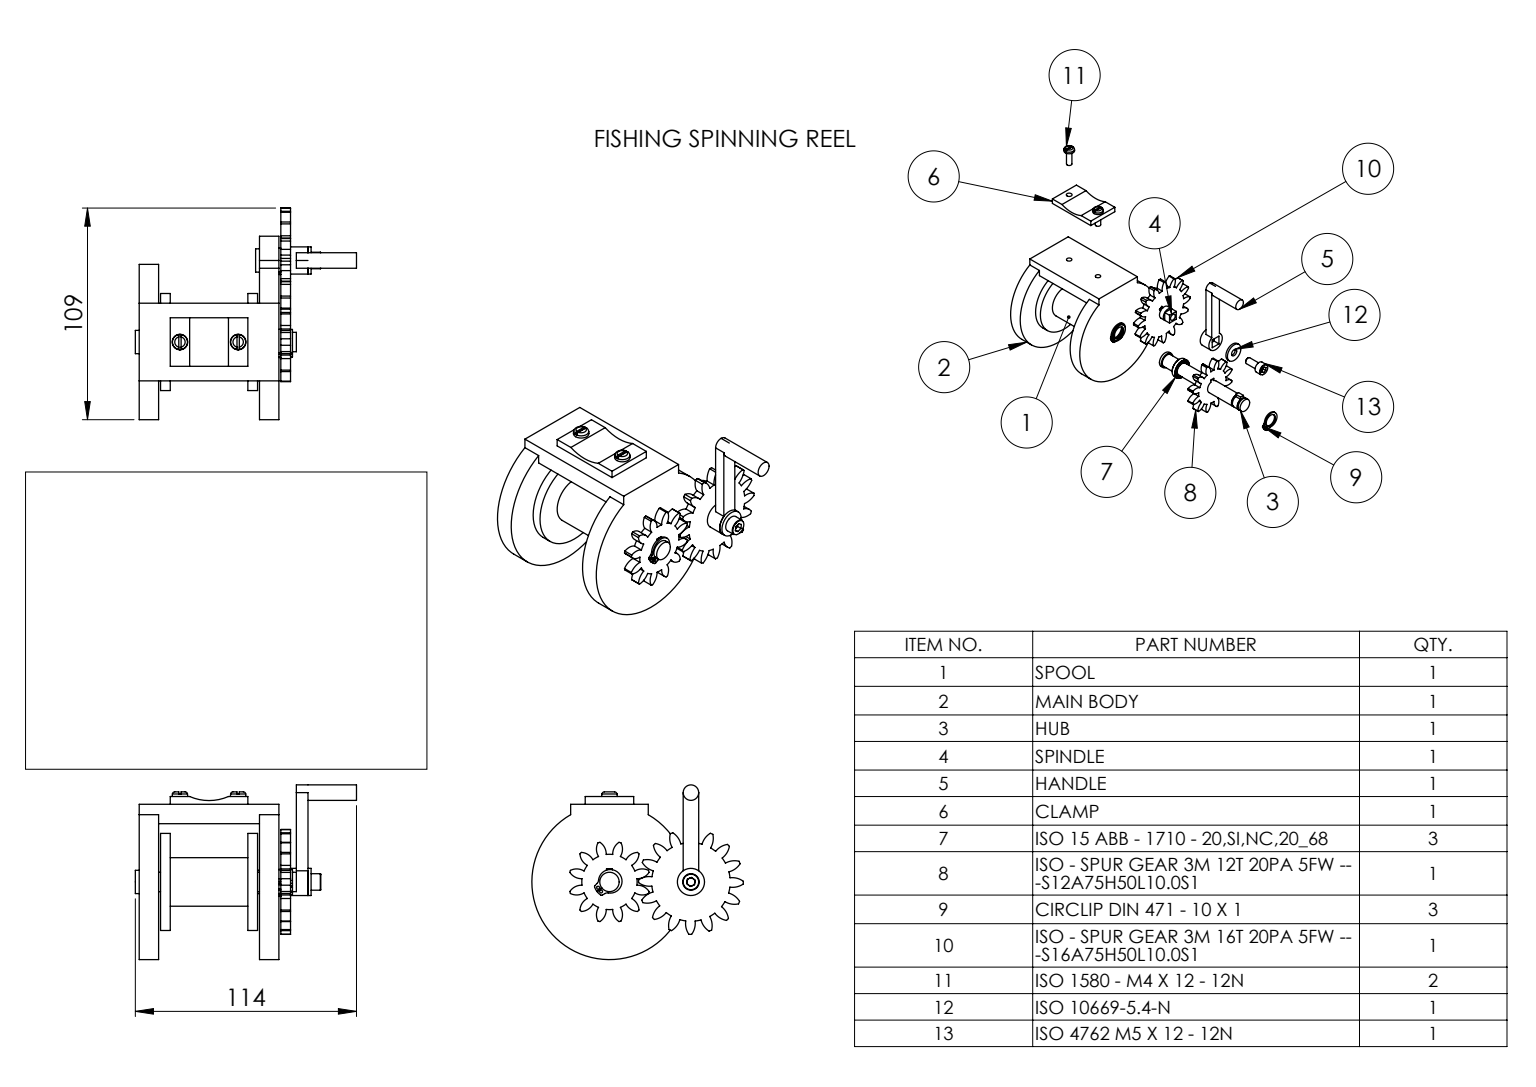
ISO-10303-21;
HEADER;
FILE_DESCRIPTION (('STEP AP214'),
    '1' );
FILE_NAME ('MAS-168',
    '2026-10-27T08:02:39',
    ( '' ),
    ( '' ),
    'SwSTEP 2.0',
    'SolidWorks 2026',
    '' );
FILE_SCHEMA (( 'AUTOMOTIVE_DESIGN' ));
ENDSEC;

DATA;
#1 = CARTESIAN_POINT ( 'NONE',  ( 4.999999999999999112, 8.035066368449411911, -14.88411597386720508 ) ) ;
#2 = FACE_OUTER_BOUND ( 'NONE', #4897, .T. ) ;
#3 = AXIS2_PLACEMENT_3D ( 'NONE', #7464, #2948, #5642 ) ;
#4 = AXIS2_PLACEMENT_3D ( 'NONE', #1352, #1240, #9072 ) ;
#5 = CARTESIAN_POINT ( 'NONE',  ( 0.000000000000000000, -11.14352537685160982, -19.60720892790264713 ) ) ;
#6 = PLANE ( 'NONE',  #3841 ) ;
#7 = ORIENTED_EDGE ( 'NONE', *, *, #8174, .F. ) ;
#8 = CYLINDRICAL_SURFACE ( 'NONE', #3786, 14.24900000001425227 ) ;
#9 = CARTESIAN_POINT ( 'NONE',  ( -36.00100000000000477, 0.000000000000000000, -41.99999999999999289 ) ) ;
#10 = ORIENTED_EDGE ( 'NONE', *, *, #7633, .F. ) ;
#11 = LINE ( 'NONE', #10463, #885 ) ;
#12 = UNCERTAINTY_MEASURE_WITH_UNIT (LENGTH_MEASURE( 1.000000000000000082E-05 ), #6900, 'distance_accuracy_value', 'NONE');
#13 = ORIENTED_EDGE ( 'NONE', *, *, #11735, .F. ) ;
#14 = CIRCLE ( 'NONE', #9018, 40.00000000000000711 ) ;
#15 = AXIS2_PLACEMENT_3D ( 'NONE', #471, #2401, #339 ) ;
#16 = EDGE_CURVE ( 'NONE', #8654, #9068, #398, .T. ) ;
#17 = SURFACE_STYLE_FILL_AREA ( #6591 ) ;
#18 = APPLICATION_CONTEXT ( 'automotive_design' ) ;
#19 = DIRECTION ( 'NONE',  ( -0.000000000000000000, 1.000000000000000000, -0.000000000000000000 ) ) ;
#20 = CARTESIAN_POINT ( 'NONE',  ( 0.000000000000000000, 0.000000000000000000, 0.000000000000000000 ) ) ;
#21 =( GEOMETRIC_REPRESENTATION_CONTEXT ( 3 ) GLOBAL_UNCERTAINTY_ASSIGNED_CONTEXT ( ( #3529 ) ) GLOBAL_UNIT_ASSIGNED_CONTEXT ( ( #3001, #9758, #2180 ) ) REPRESENTATION_CONTEXT ( 'NONE', 'WORKASPACE' ) );
#22 = DIRECTION ( 'NONE',  ( -1.000000000000000000, 0.000000000000000000, 0.000000000000000000 ) ) ;
#23 = FACE_BOUND ( 'NONE', #5725, .T. ) ;
#24 = AXIS2_PLACEMENT_3D ( 'NONE', #11957, #9116, #6050 ) ;
#25 = CIRCLE ( 'NONE', #9413, 20.24900000002024925 ) ;
#26 = VERTEX_POINT ( 'NONE', #5218 ) ;
#27 = EDGE_LOOP ( 'NONE', ( #3716, #7736, #9091, #8420 ) ) ;
#28 = VECTOR ( 'NONE', #1970, 1000.000000000000000 ) ;
#29 = CYLINDRICAL_SURFACE ( 'NONE', #9817, 4.799999999999999822 ) ;
#30 = AXIS2_PLACEMENT_3D ( 'NONE', #1488, #11904, #1413 ) ;
#31 = VERTEX_POINT ( 'NONE', #9797 ) ;
#32 = DIRECTION ( 'NONE',  ( 1.000000000000000000, -0.000000000000000000, 0.000000000000000000 ) ) ;
#33 = SHAPE_DEFINITION_REPRESENTATION ( #1615, #7946 ) ;
#34 = ORIENTED_EDGE ( 'NONE', *, *, #1883, .F. ) ;
#35 = ADVANCED_FACE ( 'NONE', ( #6155 ), #7977, .T. ) ;
#36 = AXIS2_PLACEMENT_3D ( 'NONE', #6295, #7112, #8236 ) ;
#37 = VECTOR ( 'NONE', #10938, 1000.000000000000000 ) ;
#38 = EDGE_CURVE ( 'NONE', #10710, #279, #12151, .T. ) ;
#39 = AXIS2_PLACEMENT_3D ( 'NONE', #8335, #2568, #9339 ) ;
#40 = ORIENTED_EDGE ( 'NONE', *, *, #10982, .T. ) ;
#41 = AXIS2_PLACEMENT_3D ( 'NONE', #9780, #4085, #382 ) ;
#42 = EDGE_CURVE ( 'NONE', #9980, #7044, #6787, .T. ) ;
#43 = ORIENTED_EDGE ( 'NONE', *, *, #3948, .F. ) ;
#44 = CARTESIAN_POINT ( 'NONE',  ( 4.999999999999999112, 22.37914155802281257, 2.791921004064645384 ) ) ;
#45 = DIRECTION ( 'NONE',  ( 0.03086419753086420623, -0.9995235871707959241, 0.000000000000000000 ) ) ;
#46 = DIRECTION ( 'NONE',  ( 0.000000000000000000, 0.000000000000000000, -1.000000000000000000 ) ) ;
#47 = DIRECTION ( 'NONE',  ( 0.000000000000000000, 0.000000000000000000, -1.000000000000000000 ) ) ;
#48 = ORIENTED_EDGE ( 'NONE', *, *, #3948, .T. ) ;
#50 = CYLINDRICAL_SURFACE ( 'NONE', #10960, 20.24900000002024569 ) ;
#49 =( GEOMETRIC_REPRESENTATION_CONTEXT ( 3 ) GLOBAL_UNCERTAINTY_ASSIGNED_CONTEXT ( ( #7777 ) ) GLOBAL_UNIT_ASSIGNED_CONTEXT ( ( #2594, #966, #4784 ) ) REPRESENTATION_CONTEXT ( 'NONE', 'WORKASPACE' ) );
#51 = CIRCLE ( 'NONE', #4842, 5.525000000000000355 ) ;
#52 = ORIENTED_EDGE ( 'NONE', *, *, #6778, .T. ) ;
#53 = CIRCLE ( 'NONE', #7047, 9.600000000009602630 ) ;
#54 = CIRCLE ( 'NONE', #10234, 3.873645755336797780 ) ;
#55 = ORIENTED_EDGE ( 'NONE', *, *, #1807, .F. ) ;
#56 = DIRECTION ( 'NONE',  ( 1.000000000000000000, 0.000000000000000000, 0.000000000000000000 ) ) ;
#57 = ORIENTED_EDGE ( 'NONE', *, *, #11975, .F. ) ;
#58 = DIRECTION ( 'NONE',  ( 0.000000000000000000, 0.000000000000000000, -1.000000000000000000 ) ) ;
#59 = ADVANCED_FACE ( 'NONE', ( #10781 ), #4214, .F. ) ;
#60 = EDGE_CURVE ( 'NONE', #6322, #1163, #6180, .T. ) ;
#61 = AXIS2_PLACEMENT_3D ( 'NONE', #4536, #722, #776 ) ;
#62 = VECTOR ( 'NONE', #7382, 1000.000000000000000 ) ;
#63 = EDGE_CURVE ( 'NONE', #1039, #8590, #3790, .T. ) ;
#64 = VECTOR ( 'NONE', #5535, 1000.000000000000000 ) ;
#65 = DIRECTION ( 'NONE',  ( 0.000000000000000000, 0.6828850436591804574, 0.7305258497456468270 ) ) ;
#66 = VECTOR ( 'NONE', #9457, 1000.000000000000000 ) ;
#67 = DIRECTION ( 'NONE',  ( 0.000000000000000000, 0.000000000000000000, -1.000000000000000000 ) ) ;
#68 = DIRECTION ( 'NONE',  ( -1.000000000000000000, -3.903127820947815962E-18, 0.000000000000000000 ) ) ;
#69 = ORIENTED_EDGE ( 'NONE', *, *, #8618, .F. ) ;
#70 = LINE ( 'NONE', #2883, #8880 ) ;
#71 =( LENGTH_UNIT ( ) NAMED_UNIT ( * ) SI_UNIT ( .MILLI., .METRE. ) );
#72 = CARTESIAN_POINT ( 'NONE',  ( 0.000000000000000000, -20.13931372320393010, 5.950465759858794002 ) ) ;
#73 = CARTESIAN_POINT ( 'NONE',  ( 37.00000000000000711, 6.799999999999998046, 1.500000000000000000 ) ) ;
#74 = EDGE_CURVE ( 'NONE', #10051, #9763, #2189, .T. ) ;
#75 = AXIS2_PLACEMENT_3D ( 'NONE', #10633, #5941, #1246 ) ;
#76 = ORIENTED_EDGE ( 'NONE', *, *, #9297, .F. ) ;
#77 = FACE_BOUND ( 'NONE', #651, .T. ) ;
#78 = EDGE_CURVE ( 'NONE', #474, #1066, #6869, .T. ) ;
#79 = DIRECTION ( 'NONE',  ( -1.000000000000000000, 0.000000000000000000, 0.000000000000000000 ) ) ;
#80 = CARTESIAN_POINT ( 'NONE',  ( 50.00005079999999680, 0.000000000000000000, 5.000000000000000000 ) ) ;
#81 = CARTESIAN_POINT ( 'NONE',  ( 2.499999999999999556, 22.05152472667151642, -15.57980286237449619 ) ) ;
#82 = EDGE_LOOP ( 'NONE', ( #2699, #3221, #1279, #723 ) ) ;
#83 = LINE ( 'NONE', #947, #2363 ) ;
#84 = CARTESIAN_POINT ( 'NONE',  ( 36.00000000000000711, -3.606021680338235225, -38.83193945118931367 ) ) ;
#85 = EDGE_LOOP ( 'NONE', ( #11656, #7986, #6514, #6024 ) ) ;
#86 = DIRECTION ( 'NONE',  ( 1.000000000000000000, -0.000000000000000000, -0.000000000000000000 ) ) ;
#87 = EDGE_CURVE ( 'NONE', #5401, #10239, #7657, .T. ) ;
#88 = VERTEX_POINT ( 'NONE', #10671 ) ;
#89 = AXIS2_PLACEMENT_3D ( 'NONE', #7473, #7293, #11207 ) ;
#90 = DIRECTION ( 'NONE',  ( -1.000000000000000000, -0.000000000000000000, -0.000000000000000000 ) ) ;
#91 = CARTESIAN_POINT ( 'NONE',  ( 3.098410542199072637, -7.060458129626440815, -1.000000000000000000 ) ) ;
#92 = DIRECTION ( 'NONE',  ( 1.000000000000000000, -0.000000000000000000, -0.000000000000000000 ) ) ;
#93 = CARTESIAN_POINT ( 'NONE',  ( 26.00000000000000355, 0.000000000000000000, -41.99999999999999289 ) ) ;
#94 = EDGE_LOOP ( 'NONE', ( #11994, #4647, #11472, #6806 ) ) ;
#95 = ORIENTED_EDGE ( 'NONE', *, *, #5318, .F. ) ;
#96 = VECTOR ( 'NONE', #10392, 1000.000000000000000 ) ;
#97 =( NAMED_UNIT ( * ) SI_UNIT ( $, .STERADIAN. ) SOLID_ANGLE_UNIT ( ) );
#98 = ORIENTED_EDGE ( 'NONE', *, *, #8688, .T. ) ;
#99 = DIRECTION ( 'NONE',  ( 0.000000000000000000, 0.6828850436591804574, 0.7305258497456468270 ) ) ;
#100 = PRODUCT_CONTEXT ( 'NONE', #11984, 'mechanical' ) ;
#101 = EDGE_LOOP ( 'NONE', ( #11163, #3779, #6204, #11294 ) ) ;
#102 = VERTEX_POINT ( 'NONE', #11771 ) ;
#103 = VERTEX_POINT ( 'NONE', #3228 ) ;
#104 = DIRECTION ( 'NONE',  ( -1.000000000000000000, -0.000000000000000000, 0.000000000000000000 ) ) ;
#105 = LINE ( 'NONE', #3865, #7814 ) ;
#106 = CARTESIAN_POINT ( 'NONE',  ( -31.74999999999995737, 5.204748896376250699E-16, -4.250000000000000000 ) ) ;
#107 = DIRECTION ( 'NONE',  ( -1.000000000000000000, 0.000000000000000000, -0.000000000000000000 ) ) ;
#108 = EDGE_CURVE ( 'NONE', #8484, #432, #5151, .T. ) ;
#109 = ORIENTED_EDGE ( 'NONE', *, *, #4761, .F. ) ;
#110 = FACE_OUTER_BOUND ( 'NONE', #7615, .T. ) ;
#111 = EDGE_LOOP ( 'NONE', ( #11683, #9345, #10603, #11669 ) ) ;
#112 = ADVANCED_FACE ( 'NONE', ( #8980 ), #4043, .T. ) ;
#113 = SURFACE_STYLE_FILL_AREA ( #10791 ) ;
#114 = VERTEX_POINT ( 'NONE', #4279 ) ;
#115 = CARTESIAN_POINT ( 'NONE',  ( -26.00000000000000355, -4.898587196589413815E-15, -40.00000000000000711 ) ) ;
#116 = ORIENTED_EDGE ( 'NONE', *, *, #4223, .F. ) ;
#117 = DIRECTION ( 'NONE',  ( 0.000000000000000000, 0.000000000000000000, 1.000000000000000000 ) ) ;
#118 = CARTESIAN_POINT ( 'NONE',  ( 2.500000000000000000, -1.178949249685213863, 2.042000000000002924 ) ) ;
#119 = EDGE_CURVE ( 'NONE', #4367, #3187, #6988, .T. ) ;
#120 = EDGE_LOOP ( 'NONE', ( #9318, #12086, #3898, #6255 ) ) ;
#121 = DIRECTION ( 'NONE',  ( 0.000000000000000000, 0.000000000000000000, 1.000000000000000000 ) ) ;
#122 = DIRECTION ( 'NONE',  ( -1.000000000000000000, 0.000000000000000000, 0.000000000000000000 ) ) ;
#123 = ORIENTED_EDGE ( 'NONE', *, *, #7333, .T. ) ;
#124 = DIRECTION ( 'NONE',  ( 0.000000000000000000, 0.000000000000000000, 1.000000000000000000 ) ) ;
#125 = EDGE_CURVE ( 'NONE', #9327, #10148, #1383, .T. ) ;
#126 = CARTESIAN_POINT ( 'NONE',  ( 0.000000000000000000, 20.13931372320388391, 5.950465759858938775 ) ) ;
#127 = EDGE_CURVE ( 'NONE', #10133, #6749, #9113, .T. ) ;
#128 = EDGE_CURVE ( 'NONE', #10292, #8107, #5580, .T. ) ;
#129 = DIRECTION ( 'NONE',  ( -1.000000000000000000, -0.000000000000000000, -0.000000000000000000 ) ) ;
#130 = VERTEX_POINT ( 'NONE', #2582 ) ;
#131 = CARTESIAN_POINT ( 'NONE',  ( 29.00000000000000000, 9.184850993605147944E-16, -49.49999999999999289 ) ) ;
#132 = PRODUCT ( 'circlip for shafts normal_din_Circlip DIN 471 - 10 x 1', 'circlip for shafts normal_din_Circlip DIN 471 - 10 x 1', '', ( #2666 ) ) ;
#133 = DIRECTION ( 'NONE',  ( -1.000000000000000000, -0.000000000000000000, -0.000000000000000000 ) ) ;
#134 = LINE ( 'NONE', #5901, #805 ) ;
#135 = EDGE_CURVE ( 'NONE', #9980, #9876, #10102, .T. ) ;
#136 = LINE ( 'NONE', #11503, #10649 ) ;
#137 = LINE ( 'NONE', #2829, #1850 ) ;
#138 = VERTEX_POINT ( 'NONE', #7349 ) ;
#139 = DIRECTION ( 'NONE',  ( 0.000000000000000000, 0.000000000000000000, 1.000000000000000000 ) ) ;
#140 = DIRECTION ( 'NONE',  ( 1.000000000000000000, 0.000000000000000000, 0.000000000000000000 ) ) ;
#141 = ORIENTED_EDGE ( 'NONE', *, *, #8217, .F. ) ;
#142 = FACE_BOUND ( 'NONE', #771, .T. ) ;
#143 = UNCERTAINTY_MEASURE_WITH_UNIT (LENGTH_MEASURE( 1.000000000000000082E-05 ), #8122, 'distance_accuracy_value', 'NONE');
#144 = ORIENTED_EDGE ( 'NONE', *, *, #7851, .F. ) ;
#145 = DIRECTION ( 'NONE',  ( 0.000000000000000000, 0.000000000000000000, -1.000000000000000000 ) ) ;
#146 = FACE_OUTER_BOUND ( 'NONE', #6316, .T. ) ;
#147 = EDGE_CURVE ( 'NONE', #5793, #9690, #7785, .T. ) ;
#148 = EDGE_CURVE ( 'NONE', #6125, #9230, #7162, .T. ) ;
#149 = DIRECTION ( 'NONE',  ( 0.000000000000000000, 0.000000000000000000, 1.000000000000000000 ) ) ;
#150 = DIRECTION ( 'NONE',  ( 1.000000000000000000, 0.000000000000000000, 0.000000000000000000 ) ) ;
#151 = ORIENTED_EDGE ( 'NONE', *, *, #5543, .T. ) ;
#152 = ORIENTED_EDGE ( 'NONE', *, *, #2116, .F. ) ;
#153 = EDGE_LOOP ( 'NONE', ( #1044, #6924 ) ) ;
#154 = SURFACE_STYLE_USAGE ( .BOTH. , #911 ) ;
#155 = SHAPE_DEFINITION_REPRESENTATION ( #437, #678 ) ;
#156 = ORIENTED_EDGE ( 'NONE', *, *, #8748, .T. ) ;
#157 = ORIENTED_EDGE ( 'NONE', *, *, #3999, .F. ) ;
#158 = ORIENTED_EDGE ( 'NONE', *, *, #10534, .F. ) ;
#159 = PLANE ( 'NONE',  #4576 ) ;
#160 = FACE_OUTER_BOUND ( 'NONE', #3496, .T. ) ;
#161 = CARTESIAN_POINT ( 'NONE',  ( 0.000000000000000000, 0.000000000000000000, 0.000000000000000000 ) ) ;
#162 = DIRECTION ( 'NONE',  ( 1.000000000000000000, 0.000000000000000000, 0.000000000000000000 ) ) ;
#163 = ORIENTED_EDGE ( 'NONE', *, *, #2128, .T. ) ;
#164 = CARTESIAN_POINT ( 'NONE',  ( 10.00000000000000000, 44.00000000000001421, -12.50000000000000000 ) ) ;
#165 = EDGE_LOOP ( 'NONE', ( #11428, #11250, #3782, #590 ) ) ;
#166 = EDGE_LOOP ( 'NONE', ( #4533, #1972 ) ) ;
#168 = DIRECTION ( 'NONE',  ( 0.000000000000000000, 0.000000000000000000, 1.000000000000000000 ) ) ;
#167 = AXIS2_PLACEMENT_3D ( 'NONE', #171, #5883, #6935 ) ;
#169 = CIRCLE ( 'NONE', #368, 3.873645755336797780 ) ;
#170 = VERTEX_POINT ( 'NONE', #7231 ) ;
#171 = CARTESIAN_POINT ( 'NONE',  ( 1.500000000000001332, 0.000000000000000000, 0.000000000000000000 ) ) ;
#172 = VECTOR ( 'NONE', #10661, 1000.000000000000000 ) ;
#173 = CARTESIAN_POINT ( 'NONE',  ( 2.500000000000000000, -1.768423874527823791, -1.020999999999998353 ) ) ;
#174 = EDGE_CURVE ( 'NONE', #11053, #10042, #2785, .T. ) ;
#175 = CIRCLE ( 'NONE', #11932, 27.00000000002699707 ) ;
#176 = ORIENTED_EDGE ( 'NONE', *, *, #434, .T. ) ;
#177 = CLOSED_SHELL ( 'NONE', ( #10284, #2336, #8766, #4424, #8491, #9078, #4920, #2783, #9249, #727, #1702, #2014, #7994, #8544, #7366, #12201, #5608, #5505, #10582, #11708, #6045, #8749, #2274, #6335, #7524, #5095, #6706, #112, #3625, #728, #7634, #6314, #6863, #8461, #9912, #6936, #3075, #7445, #11950, #5150, #5319, #7411, #10495, #2256, #1343, #9815, #12107, #8150, #5564, #11571, #10132, #3776, #7922, #4726, #8290, #2161, #3112, #11868, #8305, #4757, #8516, #1346, #525, #10969, #10935, #8135, #12114, #7185, #9760, #8007, #2667, #5107, #4369, #5486, #6938, #820, #1296 ) ) ;
#178 = DIRECTION ( 'NONE',  ( -1.000000000000000000, 0.000000000000000000, 0.000000000000000000 ) ) ;
#179 = DIRECTION ( 'NONE',  ( 0.000000000000000000, 0.000000000000000000, 1.000000000000000000 ) ) ;
#180 = ORIENTED_EDGE ( 'NONE', *, *, #4930, .T. ) ;
#181 = CYLINDRICAL_SURFACE ( 'NONE', #468, 5.000000000000004441 ) ;
#182 = SURFACE_STYLE_USAGE ( .BOTH. , #5944 ) ;
#183 = CARTESIAN_POINT ( 'NONE',  ( 0.000000000000000000, -22.05152472667118957, -15.57980286237495626 ) ) ;
#184 = DIRECTION ( 'NONE',  ( 1.000000000000000000, 0.000000000000000000, 0.000000000000000000 ) ) ;
#185 = VERTEX_POINT ( 'NONE', #1476 ) ;
#186 = FACE_OUTER_BOUND ( 'NONE', #7398, .T. ) ;
#187 = VECTOR ( 'NONE', #9799, 999.9999999999998863 ) ;
#188 = CIRCLE ( 'NONE', #6974, 7.500000000000000888 ) ;
#189 = EDGE_CURVE ( 'NONE', #3572, #7704, #8788, .T. ) ;
#190 = AXIS2_PLACEMENT_3D ( 'NONE', #3113, #5922, #4971 ) ;
#191 = EDGE_CURVE ( 'NONE', #922, #11041, #11147, .T. ) ;
#192 = EDGE_CURVE ( 'NONE', #3603, #3952, #2381, .T. ) ;
#193 = DIRECTION ( 'NONE',  ( -1.000000000000000000, -0.000000000000000000, -0.000000000000000000 ) ) ;
#194 = CARTESIAN_POINT ( 'NONE',  ( 51.00000000000000000, -3.499999999999998668, -45.49999999999998579 ) ) ;
#195 = DIRECTION ( 'NONE',  ( 0.000000000000000000, 0.000000000000000000, 1.000000000000000000 ) ) ;
#196 = DIRECTION ( 'NONE',  ( 0.000000000000000000, 0.000000000000000000, 1.000000000000000000 ) ) ;
#197 = CIRCLE ( 'NONE', #11173, 2.000000000000000000 ) ;
#198 = EDGE_LOOP ( 'NONE', ( #4927, #6870, #4753, #5176, #4314 ) ) ;
#199 = DIRECTION ( 'NONE',  ( -1.000000000000000000, -0.000000000000000000, 0.000000000000000000 ) ) ;
#200 = DIRECTION ( 'NONE',  ( 0.000000000000000000, 0.000000000000000000, 1.000000000000000000 ) ) ;
#201 = AXIS2_PLACEMENT_3D ( 'NONE', #9324, #9448, #3624 ) ;
#202 = ORIENTED_EDGE ( 'NONE', *, *, #9372, .F. ) ;
#203 = CYLINDRICAL_SURFACE ( 'NONE', #8088, 7.500000000000000000 ) ;
#204 = ORIENTED_EDGE ( 'NONE', *, *, #38, .F. ) ;
#205 = DIRECTION ( 'NONE',  ( 0.000000000000000000, 0.000000000000000000, 1.000000000000000000 ) ) ;
#206 = VECTOR ( 'NONE', #6495, 1000.000000000000000 ) ;
#207 = DIRECTION ( 'NONE',  ( 1.000000000000000000, 0.000000000000000000, 0.000000000000000000 ) ) ;
#208 = CARTESIAN_POINT ( 'NONE',  ( 0.000000000000000000, -5.984728032765115557, 21.74405275335756116 ) ) ;
#209 = DIRECTION ( 'NONE',  ( 0.000000000000000000, 1.224646799147353207E-16, 1.000000000000000000 ) ) ;
#210 = CARTESIAN_POINT ( 'NONE',  ( 4.999999999999999112, -16.90755573046745752, -0.4834863907627537372 ) ) ;
#211 = ORIENTED_EDGE ( 'NONE', *, *, #8369, .F. ) ;
#212 = CARTESIAN_POINT ( 'NONE',  ( 0.000000000000000000, 0.000000000000000000, 0.000000000000000000 ) ) ;
#213 = CIRCLE ( 'NONE', #1019, 7.500000000000000888 ) ;
#214 = VERTEX_POINT ( 'NONE', #5344 ) ;
#215 = FACE_OUTER_BOUND ( 'NONE', #11653, .T. ) ;
#216 = AXIS2_PLACEMENT_3D ( 'NONE', #497, #4306, #3323 ) ;
#217 = ORIENTED_EDGE ( 'NONE', *, *, #2945, .T. ) ;
#218 = CIRCLE ( 'NONE', #406, 7.200000000007204193 ) ;
#219 = ADVANCED_FACE ( 'NONE', ( #2468 ), #6409, .F. ) ;
#220 = ADVANCED_FACE ( 'NONE', ( #5475 ), #2655, .F. ) ;
#221 = DIRECTION ( 'NONE',  ( -1.000000000000000000, -0.000000000000000000, -0.000000000000000000 ) ) ;
#222 = AXIS2_PLACEMENT_3D ( 'NONE', #3797, #9085, #2730 ) ;
#223 = ORIENTED_EDGE ( 'NONE', *, *, #8092, .T. ) ;
#224 = AXIS2_PLACEMENT_3D ( 'NONE', #1139, #4013, #1014 ) ;
#225 = FACE_OUTER_BOUND ( 'NONE', #3091, .T. ) ;
#226 = DIRECTION ( 'NONE',  ( 1.000000000000000000, 0.000000000000000000, 0.000000000000000000 ) ) ;
#227 = CIRCLE ( 'NONE', #1419, 14.24900000001425227 ) ;
#228 = AXIS2_PLACEMENT_3D ( 'NONE', #6814, #4871, #168 ) ;
#229 = LINE ( 'NONE', #3922, #9820 ) ;
#230 = CYLINDRICAL_SURFACE ( 'NONE', #1227, 7.200000000007202416 ) ;
#231 = VERTEX_POINT ( 'NONE', #3477 ) ;
#232 = ORIENTED_EDGE ( 'NONE', *, *, #10676, .F. ) ;
#233 =( NAMED_UNIT ( * ) SI_UNIT ( $, .STERADIAN. ) SOLID_ANGLE_UNIT ( ) );
#234 = ORIENTED_EDGE ( 'NONE', *, *, #9201, .F. ) ;
#235 = AXIS2_PLACEMENT_3D ( 'NONE', #1289, #9923, #1479 ) ;
#236 = DIRECTION ( 'NONE',  ( -1.000000000000000000, -3.903127820947815962E-18, 0.000000000000000000 ) ) ;
#237 = AXIS2_PLACEMENT_3D ( 'NONE', #4529, #4405, #8346 ) ;
#238 = VERTEX_POINT ( 'NONE', #12026 ) ;
#239 = DIRECTION ( 'NONE',  ( -1.000000000000000000, 0.000000000000000000, 0.000000000000000000 ) ) ;
#240 = AXIS2_PLACEMENT_3D ( 'NONE', #7909, #5962, #9852 ) ;
#241 = CARTESIAN_POINT ( 'NONE',  ( 0.000000000000000000, -21.74405275335762155, 15.58472803277448726 ) ) ;
#242 = VECTOR ( 'NONE', #2897, 1000.000000000000000 ) ;
#243 = CONICAL_SURFACE ( 'NONE', #4238, 2.500000000000002220, 1.029744260000000189 ) ;
#244 = ORIENTED_EDGE ( 'NONE', *, *, #2101, .F. ) ;
#245 = CIRCLE ( 'NONE', #10429, 20.24900000002024569 ) ;
#246 = DIRECTION ( 'NONE',  ( -1.000000000000000000, -0.000000000000000000, -0.000000000000000000 ) ) ;
#247 = DIRECTION ( 'NONE',  ( 0.000000000000000000, 0.000000000000000000, -1.000000000000000000 ) ) ;
#248 = ORIENTED_EDGE ( 'NONE', *, *, #430, .T. ) ;
#249 = FACE_OUTER_BOUND ( 'NONE', #9270, .T. ) ;
#250 = FILL_AREA_STYLE ('',( #6001 ) ) ;
#251 = LINE ( 'NONE', #9999, #3639 ) ;
#252 = DIRECTION ( 'NONE',  ( 0.000000000000000000, 0.000000000000000000, -1.000000000000000000 ) ) ;
#253 = EDGE_LOOP ( 'NONE', ( #7852, #10617, #12284, #5866 ) ) ;
#254 = DIRECTION ( 'NONE',  ( 0.000000000000000000, 0.000000000000000000, 1.000000000000000000 ) ) ;
#255 = PRODUCT_DEFINITION_FORMATION_WITH_SPECIFIED_SOURCE ( 'ANY', '', #5718, .NOT_KNOWN. ) ;
#256 = VECTOR ( 'NONE', #8139, 1000.000000000000000 ) ;
#257 = AXIS2_PLACEMENT_3D ( 'NONE', #8422, #11402, #2776 ) ;
#258 = AXIS2_PLACEMENT_3D ( 'NONE', #11179, #11120, #1690 ) ;
#259 = MANIFOLD_SOLID_BREP ( 'Cavity1', #4172 ) ;
#260 = CARTESIAN_POINT ( 'NONE',  ( -36.00000000000000000, 0.000000000000000000, 0.000000000000000000 ) ) ;
#261 = CARTESIAN_POINT ( 'NONE',  ( 14.39999999999999680, 0.000000000000000000, 0.000000000000000000 ) ) ;
#262 = DIRECTION ( 'NONE',  ( -1.000000000000000000, 0.000000000000000000, 0.000000000000000000 ) ) ;
#263 = DIRECTION ( 'NONE',  ( -1.000000000000000000, 0.000000000000000000, 0.000000000000000000 ) ) ;
#264 = ORIENTED_EDGE ( 'NONE', *, *, #11856, .T. ) ;
#265 = EDGE_CURVE ( 'NONE', #8484, #2318, #5290, .T. ) ;
#266 = CARTESIAN_POINT ( 'NONE',  ( 0.000000000000000000, 22.83261415639523406, -14.41081992069285000 ) ) ;
#267 = VECTOR ( 'NONE', #3186, 1000.000000000000114 ) ;
#268 = LINE ( 'NONE', #2137, #3626 ) ;
#269 = ORIENTED_EDGE ( 'NONE', *, *, #579, .F. ) ;
#270 = CARTESIAN_POINT ( 'NONE',  ( 25.00000000000000000, 0.000000000000000000, 0.000000000000000000 ) ) ;
#271 = ADVANCED_FACE ( 'NONE', ( #5585 ), #7380, .T. ) ;
#272 = ORIENTED_EDGE ( 'NONE', *, *, #2387, .T. ) ;
#273 = PLANE ( 'NONE',  #1206 ) ;
#274 = AXIS2_PLACEMENT_3D ( 'NONE', #11157, #11099, #1724 ) ;
#275 = CYLINDRICAL_SURFACE ( 'NONE', #8197, 9.600000000009600853 ) ;
#276 = DIRECTION ( 'NONE',  ( 0.000000000000000000, 0.000000000000000000, 1.000000000000000000 ) ) ;
#277 = CARTESIAN_POINT ( 'NONE',  ( 0.000000000000000000, 46.00000000000001421, -41.99999999999999289 ) ) ;
#278 = FACE_OUTER_BOUND ( 'NONE', #10185, .T. ) ;
#279 = VERTEX_POINT ( 'NONE', #954 ) ;
#280 = MANIFOLD_SOLID_BREP ( 'Slot', #7978 ) ;
#281 = ORIENTED_EDGE ( 'NONE', *, *, #4388, .F. ) ;
#282 = FACE_BOUND ( 'NONE', #6825, .T. ) ;
#283 = EDGE_CURVE ( 'NONE', #6930, #9343, #6993, .T. ) ;
#284 = CIRCLE ( 'NONE', #2474, 4.800000000000000711 ) ;
#285 = EDGE_CURVE ( 'NONE', #11604, #9414, #8392, .T. ) ;
#286 = ORIENTED_EDGE ( 'NONE', *, *, #128, .F. ) ;
#287 = ADVANCED_FACE ( 'NONE', ( #2841 ), #4660, .F. ) ;
#288 = ORIENTED_EDGE ( 'NONE', *, *, #12313, .F. ) ;
#289 = ORIENTED_EDGE ( 'NONE', *, *, #4474, .F. ) ;
#290 = CARTESIAN_POINT ( 'NONE',  ( -1.250000000000000000, -6.429618962271402616, -1.000000000000000000 ) ) ;
#291 = DIRECTION ( 'NONE',  ( 0.000000000000000000, 0.000000000000000000, -1.000000000000000000 ) ) ;
#292 = CIRCLE ( 'NONE', #1490, 14.24900000001425582 ) ;
#293 = PLANE ( 'NONE',  #3827 ) ;
#294 = DIRECTION ( 'NONE',  ( 0.000000000000000000, 0.000000000000000000, -1.000000000000000000 ) ) ;
#295 = EDGE_LOOP ( 'NONE', ( #1962, #11859, #3381, #7606 ) ) ;
#296 = EDGE_CURVE ( 'NONE', #558, #1455, #8477, .T. ) ;
#297 = EDGE_LOOP ( 'NONE', ( #11234, #9949, #2749, #9847 ) ) ;
#298 = ORIENTED_EDGE ( 'NONE', *, *, #9479, .T. ) ;
#299 = FACE_OUTER_BOUND ( 'NONE', #4000, .T. ) ;
#300 = CIRCLE ( 'NONE', #2904, 21.00000000002100009 ) ;
#301 = DIRECTION ( 'NONE',  ( -1.000000000000000000, 0.000000000000000000, -0.000000000000000000 ) ) ;
#302 = FACE_OUTER_BOUND ( 'NONE', #521, .T. ) ;
#303 = VERTEX_POINT ( 'NONE', #4769 ) ;
#304 = AXIS2_PLACEMENT_3D ( 'NONE', #9190, #8313, #6184 ) ;
#305 = EDGE_CURVE ( 'NONE', #9528, #2794, #2709, .T. ) ;
#306 = CARTESIAN_POINT ( 'NONE',  ( 0.000000000000000000, 0.000000000000000000, 0.000000000000000000 ) ) ;
#307 = FACE_OUTER_BOUND ( 'NONE', #11547, .T. ) ;
#308 = ORIENTED_EDGE ( 'NONE', *, *, #687, .F. ) ;
#309 = DIRECTION ( 'NONE',  ( -1.000000000000000000, -0.000000000000000000, -0.000000000000000000 ) ) ;
#310 = DIRECTION ( 'NONE',  ( 0.000000000000000000, 0.000000000000000000, 1.000000000000000000 ) ) ;
#311 = EDGE_LOOP ( 'NONE', ( #6611, #4902, #12095, #9968, #4063 ) ) ;
#312 = LINE ( 'NONE', #2306, #8963 ) ;
#313 = MANIFOLD_SOLID_BREP ( 'AdvancedHole1', #9575 ) ;
#314 = DIRECTION ( 'NONE',  ( 0.000000000000000000, 0.000000000000000000, 1.000000000000000000 ) ) ;
#315 = DIRECTION ( 'NONE',  ( 0.000000000000000000, 0.000000000000000000, -1.000000000000000000 ) ) ;
#316 = CARTESIAN_POINT ( 'NONE',  ( 45.00000000000001421, 50.00000000000000711, -46.00000000000000000 ) ) ;
#317 = VERTEX_POINT ( 'NONE', #1844 ) ;
#318 = CARTESIAN_POINT ( 'NONE',  ( 0.000000000000000000, 0.000000000000000000, 0.000000000000000000 ) ) ;
#319 = DIRECTION ( 'NONE',  ( -1.000000000000000000, -0.000000000000000000, -0.000000000000000000 ) ) ;
#320 = ORIENTED_EDGE ( 'NONE', *, *, #6145, .F. ) ;
#321 = FACE_OUTER_BOUND ( 'NONE', #6866, .T. ) ;
#322 = ORIENTED_EDGE ( 'NONE', *, *, #10069, .T. ) ;
#323 = DIRECTION ( 'NONE',  ( 0.000000000000000000, 0.000000000000000000, 1.000000000000000000 ) ) ;
#324 = EDGE_CURVE ( 'NONE', #8560, #9094, #3197, .T. ) ;
#325 = DIRECTION ( 'NONE',  ( -1.000000000000000000, -0.000000000000000000, -0.000000000000000000 ) ) ;
#326 = LINE ( 'NONE', #5141, #3967 ) ;
#327 = ADVANCED_FACE ( 'NONE', ( #7270 ), #5314, .F. ) ;
#328 = CYLINDRICAL_SURFACE ( 'NONE', #1454, 5.525000000000000355 ) ;
#329 = CARTESIAN_POINT ( 'NONE',  ( 1.000000000000000000, 4.743847875303940761E-16, -3.873645755336797780 ) ) ;
#330 = PRODUCT ( 'spindle', 'spindle', '', ( #11158 ) ) ;
#331 = VERTEX_POINT ( 'NONE', #8192 ) ;
#332 = EDGE_LOOP ( 'NONE', ( #10813, #7816, #4321, #1251 ) ) ;
#333 = CARTESIAN_POINT ( 'NONE',  ( 65.79898987322334847, -9.445087446769608850E-17, -41.99999999999998579 ) ) ;
#334 = APPLICATION_PROTOCOL_DEFINITION ( 'draft international standard', 'automotive_design', 1998, #8815 ) ;
#335 = EDGE_LOOP ( 'NONE', ( #6954, #7348, #8380, #5572, #3850, #7690, #7602, #8198 ) ) ;
#336 = ADVANCED_FACE ( 'NONE', ( #548 ), #10928, .F. ) ;
#337 = DIRECTION ( 'NONE',  ( 0.000000000000000000, 0.000000000000000000, 1.000000000000000000 ) ) ;
#338 = DIRECTION ( 'NONE',  ( 0.000000000000000000, 0.000000000000000000, 1.000000000000000000 ) ) ;
#339 = DIRECTION ( 'NONE',  ( 0.000000000000000000, 0.000000000000000000, -1.000000000000000000 ) ) ;
#340 = ADVANCED_FACE ( 'NONE', ( #2436 ), #5125, .T. ) ;
#341 = FACE_OUTER_BOUND ( 'NONE', #2342, .T. ) ;
#343 = EDGE_CURVE ( 'NONE', #6998, #4367, #6189, .T. ) ;
#342 = DIRECTION ( 'NONE',  ( 1.000000000000000000, 0.000000000000000000, 0.000000000000000000 ) ) ;
#344 = VERTEX_POINT ( 'NONE', #10994 ) ;
#345 = DIRECTION ( 'NONE',  ( -1.000000000000000000, -0.000000000000000000, -0.000000000000000000 ) ) ;
#346 = ORIENTED_EDGE ( 'NONE', *, *, #9732, .F. ) ;
#347 = ORIENTED_EDGE ( 'NONE', *, *, #6557, .F. ) ;
#348 = CARTESIAN_POINT ( 'NONE',  ( 4.999999999999999112, 14.46592441914985905, -15.22291137398907068 ) ) ;
#349 = MANIFOLD_SOLID_BREP ( 'AdvancedHole1', #10962 ) ;
#350 = CARTESIAN_POINT ( 'NONE',  ( 4.999999999999999112, 0.000000000000000000, 0.000000000000000000 ) ) ;
#351 = FACE_OUTER_BOUND ( 'NONE', #1653, .T. ) ;
#352 = EDGE_CURVE ( 'NONE', #7364, #3914, #3801, .T. ) ;
#353 = VERTEX_POINT ( 'NONE', #11740 ) ;
#354 = DIRECTION ( 'NONE',  ( -1.000000000000000000, -0.000000000000000000, -0.000000000000000000 ) ) ;
#355 = LINE ( 'NONE', #8000, #10056 ) ;
#356 = AXIS2_PLACEMENT_3D ( 'NONE', #9265, #12164, #12106 ) ;
#357 = ORIENTED_EDGE ( 'NONE', *, *, #3489, .F. ) ;
#358 = CYLINDRICAL_SURFACE ( 'NONE', #10659, 5.000000000000000000 ) ;
#359 =( LENGTH_UNIT ( ) NAMED_UNIT ( * ) SI_UNIT ( .MILLI., .METRE. ) );
#360 = DIRECTION ( 'NONE',  ( 0.000000000000000000, 0.000000000000000000, 1.000000000000000000 ) ) ;
#361 = VECTOR ( 'NONE', #839, 1000.000000000000000 ) ;
#362 = CARTESIAN_POINT ( 'NONE',  ( 42.00000000000000000, 1.908195823574506293E-17, -41.99999999999998579 ) ) ;
#363 = ORIENTED_EDGE ( 'NONE', *, *, #11948, .F. ) ;
#364 = CARTESIAN_POINT ( 'NONE',  ( 42.00000000000000000, 3.183245106666225510, -38.14423151746819229 ) ) ;
#365 = ADVANCED_FACE ( 'NONE', ( #11915 ), #3321, .T. ) ;
#366 = EDGE_CURVE ( 'NONE', #11478, #710, #6798, .T. ) ;
#367 = AXIS2_PLACEMENT_3D ( 'NONE', #1541, #8125, #8179 ) ;
#368 = AXIS2_PLACEMENT_3D ( 'NONE', #1356, #11728, #9996 ) ;
#369 = PRESENTATION_STYLE_ASSIGNMENT (( #5006 ) ) ;
#370 = DIRECTION ( 'NONE',  ( 0.000000000000000000, 0.3826834323650840641, 0.9238795325112890700 ) ) ;
#371 = CARTESIAN_POINT ( 'NONE',  ( 42.00000000000000000, 0.000000000000000000, 1.500000000000000000 ) ) ;
#372 = CARTESIAN_POINT ( 'NONE',  ( -2.000000000000000000, -6.429618962271402616, 0.000000000000000000 ) ) ;
#373 = EDGE_LOOP ( 'NONE', ( #1534, #3333 ) ) ;
#374 = ORIENTED_EDGE ( 'NONE', *, *, #7609, .T. ) ;
#375 = DIRECTION ( 'NONE',  ( 0.000000000000000000, 0.000000000000000000, 1.000000000000000000 ) ) ;
#376 = CARTESIAN_POINT ( 'NONE',  ( 4.999999999999999112, -13.85025647830044271, -17.79862902732279650 ) ) ;
#377 = CIRCLE ( 'NONE', #2768, 5.750000000000000000 ) ;
#378 = ORIENTED_EDGE ( 'NONE', *, *, #265, .F. ) ;
#379 = CARTESIAN_POINT ( 'NONE',  ( 6.080745460913608902, 0.5192545390863916310, -1.000000000000000000 ) ) ;
#380 = AXIS2_PLACEMENT_3D ( 'NONE', #8436, #6808, #10487 ) ;
#381 = ORIENTED_EDGE ( 'NONE', *, *, #191, .T. ) ;
#382 = DIRECTION ( 'NONE',  ( 0.000000000000000000, 0.9238795325112878487, -0.3826834323650872283 ) ) ;
#383 = VECTOR ( 'NONE', #1264, 1000.000000000000000 ) ;
#384 = SURFACE_STYLE_FILL_AREA ( #2384 ) ;
#385 = CARTESIAN_POINT ( 'NONE',  ( 2.499999999999998668, 4.916402349214870071, -20.41639017900854469 ) ) ;
#386 = CIRCLE ( 'NONE', #11561, 7.200000000007202416 ) ;
#387 = AXIS2_PLACEMENT_3D ( 'NONE', #11303, #6559, #3504 ) ;
#388 = CYLINDRICAL_SURFACE ( 'NONE', #4436, 7.200000000007202416 ) ;
#389 = DIRECTION ( 'NONE',  ( 0.000000000000000000, 0.000000000000000000, -1.000000000000000000 ) ) ;
#390 = ORIENTED_EDGE ( 'NONE', *, *, #3924, .T. ) ;
#391 = CARTESIAN_POINT ( 'NONE',  ( 2.399999999999999467, 4.898587196589413815E-16, 4.000000000000000000 ) ) ;
#392 = EDGE_LOOP ( 'NONE', ( #8569, #7501, #1729, #4037 ) ) ;
#393 = DIRECTION ( 'NONE',  ( 1.000000000000000000, 0.000000000000000000, 0.000000000000000000 ) ) ;
#394 = VERTEX_POINT ( 'NONE', #4251 ) ;
#395 = AXIS2_PLACEMENT_3D ( 'NONE', #290, #10783, #1338 ) ;
#396 = EDGE_CURVE ( 'NONE', #709, #1692, #8083, .T. ) ;
#397 = CIRCLE ( 'NONE', #9396, 7.200000000007201528 ) ;
#398 = LINE ( 'NONE', #8798, #3386 ) ;
#399 = PLANE ( 'NONE',  #10583 ) ;
#400 = CARTESIAN_POINT ( 'NONE',  ( 0.09947414737648539729, 0.5999999999999997558, -3.189051013155320469 ) ) ;
#401 = FACE_OUTER_BOUND ( 'NONE', #670, .T. ) ;
#402 = CARTESIAN_POINT ( 'NONE',  ( 0.000000000000000000, -16.90755573046745752, -0.4834863907627537372 ) ) ;
#403 = VERTEX_POINT ( 'NONE', #11063 ) ;
#404 = VECTOR ( 'NONE', #11917, 1000.000000000000000 ) ;
#405 = LINE ( 'NONE', #1345, #2435 ) ;
#406 = AXIS2_PLACEMENT_3D ( 'NONE', #7256, #11054, #2485 ) ;
#407 = ORIENTED_EDGE ( 'NONE', *, *, #7533, .T. ) ;
#408 = EDGE_CURVE ( 'NONE', #2942, #11480, #10780, .T. ) ;
#409 = SURFACE_STYLE_FILL_AREA ( #4344 ) ;
#410 = ORIENTED_EDGE ( 'NONE', *, *, #5322, .F. ) ;
#411 = DIRECTION ( 'NONE',  ( -1.000000000000000000, 0.000000000000000000, 0.000000000000000000 ) ) ;
#412 = ADVANCED_FACE ( 'NONE', ( #1443 ), #5260, .T. ) ;
#413 = LINE ( 'NONE', #4060, #11148 ) ;
#414 = EDGE_CURVE ( 'NONE', #11497, #7805, #1388, .T. ) ;
#415 = CIRCLE ( 'NONE', #9610, 7.200000000007202416 ) ;
#416 = AXIS2_PLACEMENT_3D ( 'NONE', #8285, #1835, #8338 ) ;
#417 = VECTOR ( 'NONE', #8737, 1000.000000000000000 ) ;
#418 = AXIS2_PLACEMENT_3D ( 'NONE', #10477, #3731, #9491 ) ;
#419 = FACE_OUTER_BOUND ( 'NONE', #4196, .T. ) ;
#420 = VERTEX_POINT ( 'NONE', #12297 ) ;
#421 = FACE_OUTER_BOUND ( 'NONE', #899, .T. ) ;
#422 = AXIS2_PLACEMENT_3D ( 'NONE', #6109, #1403, #7981 ) ;
#423 = ORIENTED_EDGE ( 'NONE', *, *, #10700, .T. ) ;
#424 = AXIS2_PLACEMENT_3D ( 'NONE', #3329, #7021, #7141 ) ;
#425 =( LENGTH_UNIT ( ) NAMED_UNIT ( * ) SI_UNIT ( .MILLI., .METRE. ) );
#426 = AXIS2_PLACEMENT_3D ( 'NONE', #93, #5779, #1149 ) ;
#427 = DIRECTION ( 'NONE',  ( 1.000000000000000000, -0.000000000000000000, -0.000000000000000000 ) ) ;
#428 = AXIS2_PLACEMENT_3D ( 'NONE', #10140, #7338, #1516 ) ;
#429 = DIRECTION ( 'NONE',  ( -1.000000000000000000, -0.000000000000000000, -0.000000000000000000 ) ) ;
#430 = EDGE_CURVE ( 'NONE', #4941, #709, #2995, .T. ) ;
#432 = VERTEX_POINT ( 'NONE', #10181 ) ;
#431 = ADVANCED_FACE ( 'NONE', ( #738 ), #686, .F. ) ;
#433 = CARTESIAN_POINT ( 'NONE',  ( 29.00000000000000000, 0.000000000000000000, -34.49999999999999289 ) ) ;
#434 = EDGE_CURVE ( 'NONE', #4082, #4193, #4789, .T. ) ;
#435 = AXIS2_PLACEMENT_3D ( 'NONE', #4528, #8295, #2526 ) ;
#436 = CIRCLE ( 'NONE', #11425, 4.799999999999998934 ) ;
#437 = PRODUCT_DEFINITION_SHAPE ( 'NONE', 'NONE',  #7937 ) ;
#438 = DIRECTION ( 'NONE',  ( 0.000000000000000000, 0.000000000000000000, 1.000000000000000000 ) ) ;
#439 = VECTOR ( 'NONE', #9841, 1000.000000000000000 ) ;
#440 = SURFACE_SIDE_STYLE ('',( #8017 ) ) ;
#441 = CARTESIAN_POINT ( 'NONE',  ( 46.00000000000000000, 3.500000000000001332, -38.49999999999998579 ) ) ;
#442 = CARTESIAN_POINT ( 'NONE',  ( -26.00000000000000355, 30.00000000000000711, 20.00000000000001066 ) ) ;
#443 = DIRECTION ( 'NONE',  ( 0.000000000000000000, 0.000000000000000000, 1.000000000000000000 ) ) ;
#444 = ORIENTED_EDGE ( 'NONE', *, *, #8688, .F. ) ;
#445 = ORIENTED_EDGE ( 'NONE', *, *, #2739, .T. ) ;
#446 = DIRECTION ( 'NONE',  ( -1.000000000000000000, -0.000000000000000000, -0.000000000000000000 ) ) ;
#447 = EDGE_CURVE ( 'NONE', #1975, #4496, #2545, .T. ) ;
#448 = LINE ( 'NONE', #6956, #1041 ) ;
#449 = EDGE_CURVE ( 'NONE', #4349, #4914, #3593, .T. ) ;
#450 = ORIENTED_EDGE ( 'NONE', *, *, #9313, .T. ) ;
#451 = VERTEX_POINT ( 'NONE', #614 ) ;
#452 = FACE_BOUND ( 'NONE', #11698, .T. ) ;
#453 = AXIS2_PLACEMENT_3D ( 'NONE', #10970, #2408, #533 ) ;
#454 = AXIS2_PLACEMENT_3D ( 'NONE', #10757, #4010, #11636 ) ;
#455 = ORIENTED_EDGE ( 'NONE', *, *, #11034, .T. ) ;
#456 = FACE_OUTER_BOUND ( 'NONE', #2314, .T. ) ;
#457 = AXIS2_PLACEMENT_3D ( 'NONE', #6194, #7953, #1192 ) ;
#458 = CARTESIAN_POINT ( 'NONE',  ( 46.00000000000000000, 6.123233995736773185E-16, -46.99999999999999289 ) ) ;
#459 = CIRCLE ( 'NONE', #3072, 12.50000000000000000 ) ;
#460 = DIRECTION ( 'NONE',  ( -1.000000000000000000, -0.000000000000000000, 0.000000000000000000 ) ) ;
#461 = CYLINDRICAL_SURFACE ( 'NONE', #12016, 21.00000000002100009 ) ;
#462 = ORIENTED_EDGE ( 'NONE', *, *, #746, .F. ) ;
#463 = EDGE_CURVE ( 'NONE', #1857, #10975, #10577, .T. ) ;
#464 = LINE ( 'NONE', #3290, #7821 ) ;
#465 = ORIENTED_EDGE ( 'NONE', *, *, #560, .F. ) ;
#466 = SURFACE_STYLE_FILL_AREA ( #10901 ) ;
#467 = EDGE_LOOP ( 'NONE', ( #2592, #10546 ) ) ;
#468 = AXIS2_PLACEMENT_3D ( 'NONE', #2246, #10558, #8702 ) ;
#469 = DIRECTION ( 'NONE',  ( 0.000000000000000000, 0.000000000000000000, 1.000000000000000000 ) ) ;
#470 = DIRECTION ( 'NONE',  ( 0.03086419753086420623, -0.9995235871707959241, 0.000000000000000000 ) ) ;
#471 = CARTESIAN_POINT ( 'NONE',  ( 1.399999999999999689, 0.000000000000000000, -7.399999999999999467 ) ) ;
#472 = CARTESIAN_POINT ( 'NONE',  ( 37.00000000000000711, 0.000000000000000000, 0.000000000000000000 ) ) ;
#473 = DIRECTION ( 'NONE',  ( -1.000000000000000000, 0.000000000000000000, 0.000000000000000000 ) ) ;
#474 = VERTEX_POINT ( 'NONE', #3689 ) ;
#475 = VECTOR ( 'NONE', #9225, 1000.000000000000000 ) ;
#476 = DIRECTION ( 'NONE',  ( 0.000000000000000000, 0.000000000000000000, 1.000000000000000000 ) ) ;
#477 = VERTEX_POINT ( 'NONE', #2804 ) ;
#478 = DIRECTION ( 'NONE',  ( -1.000000000000000000, 0.000000000000000000, 0.000000000000000000 ) ) ;
#479 = ORIENTED_EDGE ( 'NONE', *, *, #9679, .F. ) ;
#480 = CARTESIAN_POINT ( 'NONE',  ( -38.00000000000000000, 0.000000000000000000, 0.000000000000000000 ) ) ;
#481 = CARTESIAN_POINT ( 'NONE',  ( 43.00000000000000000, -3.792354139917827993, -2.942456469932580365 ) ) ;
#482 = ORIENTED_EDGE ( 'NONE', *, *, #7502, .T. ) ;
#483 = CARTESIAN_POINT ( 'NONE',  ( 26.00000000000000355, -12.50000000000000000, -37.99671038392666134 ) ) ;
#484 = EDGE_CURVE ( 'NONE', #1854, #1927, #8266, .T. ) ;
#485 = EDGE_CURVE ( 'NONE', #331, #5149, #6388, .T. ) ;
#486 = VERTEX_POINT ( 'NONE', #7507 ) ;
#487 = DIRECTION ( 'NONE',  ( -1.000000000000000000, -0.000000000000000000, 0.000000000000000000 ) ) ;
#488 = ORIENTED_EDGE ( 'NONE', *, *, #5345, .F. ) ;
#489 = AXIS2_PLACEMENT_3D ( 'NONE', #1633, #11075, #12117 ) ;
#490 = CARTESIAN_POINT ( 'NONE',  ( 0.000000000000000000, 14.40062958310465469, -8.872489362018239234 ) ) ;
#491 = ORIENTED_EDGE ( 'NONE', *, *, #2315, .T. ) ;
#492 = CARTESIAN_POINT ( 'NONE',  ( 50.00005079999999680, 6.799999999999999822, 1.500000000000000000 ) ) ;
#493 = APPLICATION_CONTEXT ( 'automotive_design' ) ;
#494 =( LENGTH_UNIT ( ) NAMED_UNIT ( * ) SI_UNIT ( .MILLI., .METRE. ) );
#495 = EDGE_CURVE ( 'NONE', #1234, #3139, #11361, .T. ) ;
#496 = CARTESIAN_POINT ( 'NONE',  ( 0.1893088852826965152, 0.6000000000000000888, 3.298489774147015829 ) ) ;
#497 = CARTESIAN_POINT ( 'NONE',  ( 45.00000000000001421, 4.770489558936308102E-18, -41.99999999999998579 ) ) ;
#498 = EDGE_CURVE ( 'NONE', #1263, #8559, #8375, .T. ) ;
#499 = EDGE_CURVE ( 'NONE', #10309, #3410, #4192, .T. ) ;
#500 = CARTESIAN_POINT ( 'NONE',  ( 1.399999999999998579, 0.000000000000000000, 0.000000000000000000 ) ) ;
#501 = DIRECTION ( 'NONE',  ( -0.000000000000000000, 1.000000000000000000, -0.000000000000000000 ) ) ;
#502 = EDGE_CURVE ( 'NONE', #1765, #8121, #3008, .T. ) ;
#503 = EDGE_LOOP ( 'NONE', ( #1832, #534 ) ) ;
#504 = VERTEX_POINT ( 'NONE', #4500 ) ;
#505 = CARTESIAN_POINT ( 'NONE',  ( 0.7248882449525384519, -0.5999999999999994227, -3.753866745206998701 ) ) ;
#506 = SURFACE_STYLE_FILL_AREA ( #8323 ) ;
#507 = CYLINDRICAL_SURFACE ( 'NONE', #5435, 4.799999999999999822 ) ;
#508 = ORIENTED_EDGE ( 'NONE', *, *, #2896, .F. ) ;
#509 = DIRECTION ( 'NONE',  ( -1.000000000000000000, -0.000000000000000000, -0.000000000000000000 ) ) ;
#510 = ORIENTED_EDGE ( 'NONE', *, *, #3017, .F. ) ;
#511 = FACE_OUTER_BOUND ( 'NONE', #2048, .T. ) ;
#512 = ORIENTED_EDGE ( 'NONE', *, *, #3959, .T. ) ;
#513 =( LENGTH_UNIT ( ) NAMED_UNIT ( * ) SI_UNIT ( .MILLI., .METRE. ) );
#514 = PLANE ( 'NONE',  #6100 ) ;
#515 = CARTESIAN_POINT ( 'NONE',  ( 0.000000000000000000, 0.000000000000000000, 0.000000000000000000 ) ) ;
#516 = CYLINDRICAL_SURFACE ( 'NONE', #1244, 40.00000000000000711 ) ;
#517 = PRODUCT_RELATED_PRODUCT_CATEGORY ( 'part', '', ( #6127 ) ) ;
#518 = ORIENTED_EDGE ( 'NONE', *, *, #8114, .T. ) ;
#519 = LINE ( 'NONE', #4329, #5171 ) ;
#520 = DIRECTION ( 'NONE',  ( -1.000000000000000000, -0.000000000000000000, -0.000000000000000000 ) ) ;
#521 = EDGE_LOOP ( 'NONE', ( #7403, #789, #6236, #8961 ) ) ;
#522 = CARTESIAN_POINT ( 'NONE',  ( 4.999999999999999112, 8.872489362018390224, -14.40062958310456054 ) ) ;
#523 = UNCERTAINTY_MEASURE_WITH_UNIT (LENGTH_MEASURE( 1.000000000000000082E-05 ), #3240, 'distance_accuracy_value', 'NONE');
#524 = ORIENTED_EDGE ( 'NONE', *, *, #1950, .F. ) ;
#525 = ADVANCED_FACE ( 'NONE', ( #2684 ), #3746, .T. ) ;
#526 = DIRECTION ( 'NONE',  ( -1.000000000000000000, -0.000000000000000000, -0.000000000000000000 ) ) ;
#527 = ADVANCED_FACE ( 'NONE', ( #12108 ), #3217, .T. ) ;
#528 = DIRECTION ( 'NONE',  ( 0.000000000000000000, 0.000000000000000000, 1.000000000000000000 ) ) ;
#529 = DIRECTION ( 'NONE',  ( -1.000000000000000000, -0.000000000000000000, 0.000000000000000000 ) ) ;
#530 = DIRECTION ( 'NONE',  ( 1.000000000000000000, 0.000000000000000000, 0.000000000000000000 ) ) ;
#531 = FACE_BOUND ( 'NONE', #11009, .T. ) ;
#532 = ORIENTED_EDGE ( 'NONE', *, *, #567, .F. ) ;
#533 = DIRECTION ( 'NONE',  ( 0.000000000000000000, 0.000000000000000000, 1.000000000000000000 ) ) ;
#534 = ORIENTED_EDGE ( 'NONE', *, *, #8490, .T. ) ;
#535 = DIRECTION ( 'NONE',  ( 1.000000000000000000, 0.000000000000000000, 1.568609339482109940E-17 ) ) ;
#536 = VERTEX_POINT ( 'NONE', #4438 ) ;
#537 = DIRECTION ( 'NONE',  ( -1.000000000000000000, -0.000000000000000000, -0.000000000000000000 ) ) ;
#538 = FACE_OUTER_BOUND ( 'NONE', #3304, .T. ) ;
#539 = ORIENTED_EDGE ( 'NONE', *, *, #11233, .F. ) ;
#540 = ORIENTED_EDGE ( 'NONE', *, *, #2766, .F. ) ;
#541 = CARTESIAN_POINT ( 'NONE',  ( 0.000000000000000000, 0.000000000000000000, 0.000000000000000000 ) ) ;
#542 = VERTEX_POINT ( 'NONE', #11176 ) ;
#543 =( NAMED_UNIT ( * ) SI_UNIT ( $, .STERADIAN. ) SOLID_ANGLE_UNIT ( ) );
#544 = DIRECTION ( 'NONE',  ( 0.000000000000000000, 0.000000000000000000, -1.000000000000000000 ) ) ;
#545 = ORIENTED_EDGE ( 'NONE', *, *, #3935, .T. ) ;
#546 = DIRECTION ( 'NONE',  ( 0.000000000000000000, -0.3826834323650971093, 0.9238795325112837409 ) ) ;
#547 = EDGE_CURVE ( 'NONE', #11485, #10027, #10190, .T. ) ;
#548 = FACE_OUTER_BOUND ( 'NONE', #392, .T. ) ;
#549 = CARTESIAN_POINT ( 'NONE',  ( 0.3704956024625865041, 0.5999999999999998668, 3.518228334340779195 ) ) ;
#550 = DIRECTION ( 'NONE',  ( 0.000000000000000000, 0.000000000000000000, 1.000000000000000000 ) ) ;
#551 = CARTESIAN_POINT ( 'NONE',  ( 45.00000000000000000, 4.769696007084727185, 1.500000000000000000 ) ) ;
#552 = FACE_BOUND ( 'NONE', #153, .T. ) ;
#553 = ORIENTED_EDGE ( 'NONE', *, *, #10197, .F. ) ;
#554 = ORIENTED_EDGE ( 'NONE', *, *, #10262, .T. ) ;
#555 = DIRECTION ( 'NONE',  ( 0.000000000000000000, -0.9238795325112906243, 0.3826834323650805669 ) ) ;
#556 = DIRECTION ( 'NONE',  ( 1.000000000000000000, 0.000000000000000000, 0.000000000000000000 ) ) ;
#557 = CARTESIAN_POINT ( 'NONE',  ( -20.00000000000000000, 40.00000000000000711, 12.50000000000000000 ) ) ;
#558 = VERTEX_POINT ( 'NONE', #4624 ) ;
#559 = FACE_OUTER_BOUND ( 'NONE', #11903, .T. ) ;
#560 = EDGE_CURVE ( 'NONE', #11027, #12039, #1005, .T. ) ;
#561 = ORIENTED_EDGE ( 'NONE', *, *, #3933, .T. ) ;
#562 = CARTESIAN_POINT ( 'NONE',  ( 0.000000000000000000, 8.527191590521072229, 11.41582255376076027 ) ) ;
#563 = CIRCLE ( 'NONE', #1979, 9.600000000009600853 ) ;
#564 = AXIS2_PLACEMENT_3D ( 'NONE', #1557, #9139, #10182 ) ;
#565 = ADVANCED_FACE ( 'NONE', ( #4744 ), #6885, .T. ) ;
#566 = CIRCLE ( 'NONE', #7566, 21.00000000002100009 ) ;
#567 = EDGE_CURVE ( 'NONE', #11902, #11981, #6636, .T. ) ;
#568 = CARTESIAN_POINT ( 'NONE',  ( 2.499999999999999556, -26.33508479058316709, -5.955107813822780649 ) ) ;
#569 = CARTESIAN_POINT ( 'NONE',  ( 2.595115354961440524, -7.673029147243177306, 0.000000000000000000 ) ) ;
#570 = CARTESIAN_POINT ( 'NONE',  ( 4.999999999999999112, 15.22291137398921990, 14.46592441914969918 ) ) ;
#571 = DIRECTION ( 'NONE',  ( 1.000000000000000000, -0.000000000000000000, -0.000000000000000000 ) ) ;
#572 = AXIS2_PLACEMENT_3D ( 'NONE', #11910, #10065, #680 ) ;
#573 = ORIENTED_EDGE ( 'NONE', *, *, #11359, .T. ) ;
#574 = CARTESIAN_POINT ( 'NONE',  ( 51.00000000000000000, -3.499999999999998668, -38.49999999999998579 ) ) ;
#575 = LINE ( 'NONE', #164, #4417 ) ;
#576 = ORIENTED_EDGE ( 'NONE', *, *, #10600, .F. ) ;
#577 = DIRECTION ( 'NONE',  ( 0.000000000000000000, 0.000000000000000000, -1.000000000000000000 ) ) ;
#578 = ORIENTED_EDGE ( 'NONE', *, *, #2670, .T. ) ;
#579 = EDGE_CURVE ( 'NONE', #752, #1455, #7699, .T. ) ;
#580 = CIRCLE ( 'NONE', #2188, 20.24900000002024569 ) ;
#581 = DIRECTION ( 'NONE',  ( -1.000000000000000000, 0.000000000000000000, 0.000000000000000000 ) ) ;
#582 = AXIS2_PLACEMENT_3D ( 'NONE', #7871, #10854, #2285 ) ;
#583 = DIRECTION ( 'NONE',  ( 1.000000000000000000, 0.000000000000000000, 0.000000000000000000 ) ) ;
#584 = DIRECTION ( 'NONE',  ( -1.000000000000000000, 0.000000000000000000, 0.000000000000000000 ) ) ;
#585 = DIRECTION ( 'NONE',  ( -1.000000000000000000, 0.000000000000000000, 0.000000000000000000 ) ) ;
#586 = CARTESIAN_POINT ( 'NONE',  ( 42.00000000000000000, 4.817162211711309538, -40.66024322130446222 ) ) ;
#587 = EDGE_LOOP ( 'NONE', ( #7114, #3255, #8171, #7068, #1098, #2370 ) ) ;
#588 = SHAPE_REPRESENTATION ( 'socket head cap screw_iso_ISO 4762 M5 x 12 - 12N', ( #6056 ), #8443 ) ;
#589 = LINE ( 'NONE', #3484, #11033 ) ;
#590 = ORIENTED_EDGE ( 'NONE', *, *, #9258, .F. ) ;
#591 = CARTESIAN_POINT ( 'NONE',  ( 36.00000000000000711, 0.000000000000000000, -41.99999999999999289 ) ) ;
#592 = CARTESIAN_POINT ( 'NONE',  ( 36.00000000000000711, -4.104405154062230115E-16, -2.224720805914714718E-17 ) ) ;
#593 = EDGE_CURVE ( 'NONE', #6667, #1161, #5812, .T. ) ;
#595 = EDGE_CURVE ( 'NONE', #3600, #7392, #2994, .T. ) ;
#594 = ORIENTED_EDGE ( 'NONE', *, *, #7647, .F. ) ;
#596 = AXIS2_PLACEMENT_3D ( 'NONE', #7195, #3371, #9943 ) ;
#597 = DIRECTION ( 'NONE',  ( 0.000000000000000000, -6.866613759067995433E-15, 1.000000000000000000 ) ) ;
#598 = CARTESIAN_POINT ( 'NONE',  ( 33.00000000000000000, 0.000000000000000000, 0.000000000000000000 ) ) ;
#599 = CIRCLE ( 'NONE', #7003, 21.00000000002100009 ) ;
#600 = ORIENTED_EDGE ( 'NONE', *, *, #5405, .T. ) ;
#601 = DIRECTION ( 'NONE',  ( -1.000000000000000000, 0.000000000000000000, 0.000000000000000000 ) ) ;
#602 = AXIS2_PLACEMENT_3D ( 'NONE', #2827, #9653, #11378 ) ;
#603 = AXIS2_PLACEMENT_3D ( 'NONE', #7936, #5992, #9880 ) ;
#604 = ORIENTED_EDGE ( 'NONE', *, *, #12029, .T. ) ;
#605 = DIRECTION ( 'NONE',  ( 0.000000000000000000, -0.5000000000000012212, -0.8660254037844380415 ) ) ;
#606 = ORIENTED_EDGE ( 'NONE', *, *, #3795, .T. ) ;
#607 = FILL_AREA_STYLE ('',( #1683 ) ) ;
#608 = VECTOR ( 'NONE', #3199, 1000.000000000000000 ) ;
#609 = CARTESIAN_POINT ( 'NONE',  ( 36.00000000000000711, -4.104405154062230115E-16, -2.224720805914714718E-17 ) ) ;
#610 = CIRCLE ( 'NONE', #7014, 9.600000000009600853 ) ;
#611 = VERTEX_POINT ( 'NONE', #10688 ) ;
#612 = DIRECTION ( 'NONE',  ( -1.000000000000000000, -0.000000000000000000, 0.000000000000000000 ) ) ;
#613 = AXIS2_PLACEMENT_3D ( 'NONE', #3547, #857, #2536 ) ;
#614 = CARTESIAN_POINT ( 'NONE',  ( 33.00000000000000000, 0.000000000000000000, -47.19999999999998863 ) ) ;
#615 = AXIS2_PLACEMENT_3D ( 'NONE', #2148, #3107, #7677 ) ;
#616 = AXIS2_PLACEMENT_3D ( 'NONE', #161, #1107, #1158 ) ;
#617 = AXIS2_PLACEMENT_3D ( 'NONE', #7586, #7405, #757 ) ;
#618 = DIRECTION ( 'NONE',  ( 0.000000000000000000, 8.881784197001252323E-16, 1.000000000000000000 ) ) ;
#619 = CIRCLE ( 'NONE', #6640, 7.200000000007202416 ) ;
#620 = AXIS2_PLACEMENT_3D ( 'NONE', #9988, #3488, #10977 ) ;
#621 = FACE_OUTER_BOUND ( 'NONE', #9304, .T. ) ;
#622 = LINE ( 'NONE', #3508, #9651 ) ;
#623 = ORIENTED_EDGE ( 'NONE', *, *, #10422, .F. ) ;
#624 = ORIENTED_EDGE ( 'NONE', *, *, #2786, .T. ) ;
#625 = CARTESIAN_POINT ( 'NONE',  ( -25.00000000000000000, 0.000000000000000000, 0.000000000000000000 ) ) ;
#626 = DIRECTION ( 'NONE',  ( -1.000000000000000000, -0.000000000000000000, 0.000000000000000000 ) ) ;
#627 = ORIENTED_EDGE ( 'NONE', *, *, #11894, .F. ) ;
#628 = DIRECTION ( 'NONE',  ( -1.000000000000000000, -0.000000000000000000, -0.000000000000000000 ) ) ;
#629 = VERTEX_POINT ( 'NONE', #5742 ) ;
#630 = CARTESIAN_POINT ( 'NONE',  ( -31.74999999999995737, 0.000000000000000000, 0.000000000000000000 ) ) ;
#631 = COLOUR_RGB ( '',0.8941176470588234615, 0.8941176470588234615, 0.8941176470588234615 ) ;
#632 = AXIS2_PLACEMENT_3D ( 'NONE', #3534, #3664, #4664 ) ;
#633 = AXIS2_PLACEMENT_3D ( 'NONE', #8324, #9459, #7388 ) ;
#634 = AXIS2_PLACEMENT_3D ( 'NONE', #5026, #9910, #7099 ) ;
#635 = VECTOR ( 'NONE', #1004, 1000.000000000000000 ) ;
#636 =( LENGTH_UNIT ( ) NAMED_UNIT ( * ) SI_UNIT ( .MILLI., .METRE. ) );
#637 = DIRECTION ( 'NONE',  ( -1.000000000000000000, 0.000000000000000000, -0.000000000000000000 ) ) ;
#638 = ADVANCED_FACE ( 'NONE', ( #2934 ), #10626, .T. ) ;
#639 = STYLED_ITEM ( 'NONE', ( #8368 ), #8868 ) ;
#640 = CARTESIAN_POINT ( 'NONE',  ( 0.000000000000000000, 0.000000000000000000, 0.000000000000000000 ) ) ;
#641 = LINE ( 'NONE', #11202, #11025 ) ;
#642 = CIRCLE ( 'NONE', #6043, 25.00000000000000000 ) ;
#643 = PRODUCT_DEFINITION_SHAPE ( 'NONE', 'NONE',  #12365 ) ;
#644 = VERTEX_POINT ( 'NONE', #241 ) ;
#645 = EDGE_CURVE ( 'NONE', #3502, #9875, #4601, .T. ) ;
#646 = CARTESIAN_POINT ( 'NONE',  ( 37.00000000000000711, -2.432816653220593039, 4.137801726981678030 ) ) ;
#647 = AXIS2_PLACEMENT_3D ( 'NONE', #6522, #4460, #10094 ) ;
#648 = FACE_OUTER_BOUND ( 'NONE', #8532, .T. ) ;
#649 = VERTEX_POINT ( 'NONE', #173 ) ;
#650 = CARTESIAN_POINT ( 'NONE',  ( 0.2500000000000002220, 4.898587196589412829E-16, -4.000000000000000000 ) ) ;
#651 = EDGE_LOOP ( 'NONE', ( #9311, #3965, #6290, #11424, #2951, #410 ) ) ;
#652 = AXIS2_PLACEMENT_3D ( 'NONE', #2372, #5269, #556 ) ;
#653 = AXIS2_PLACEMENT_3D ( 'NONE', #10130, #1625, #8195 ) ;
#654 = AXIS2_PLACEMENT_3D ( 'NONE', #12142, #12213, #1855 ) ;
#655 = AXIS2_PLACEMENT_3D ( 'NONE', #4690, #8568, #9509 ) ;
#656 = CARTESIAN_POINT ( 'NONE',  ( 2.499999999999999556, 14.46592441914965121, 15.22291137398927141 ) ) ;
#657 = DIRECTION ( 'NONE',  ( 1.000000000000000000, 0.000000000000000000, 0.000000000000000000 ) ) ;
#658 = EDGE_CURVE ( 'NONE', #4082, #4830, #4877, .T. ) ;
#659 = PLANE ( 'NONE',  #632 ) ;
#660 = DIRECTION ( 'NONE',  ( 0.000000000000000000, 0.000000000000000000, -1.000000000000000000 ) ) ;
#661 = VERTEX_POINT ( 'NONE', #4061 ) ;
#662 = EDGE_CURVE ( 'NONE', #5342, #3842, #7885, .T. ) ;
#663 = ADVANCED_FACE ( 'NONE', ( #9634 ), #5938, .T. ) ;
#664 = DIRECTION ( 'NONE',  ( -0.000000000000000000, 1.000000000000000000, -0.000000000000000000 ) ) ;
#665 = DIRECTION ( 'NONE',  ( -1.000000000000000000, 0.000000000000000000, 0.000000000000000000 ) ) ;
#666 = EDGE_CURVE ( 'NONE', #12146, #7642, #10385, .T. ) ;
#667 = ORIENTED_EDGE ( 'NONE', *, *, #5254, .F. ) ;
#668 = CARTESIAN_POINT ( 'NONE',  ( 0.000000000000000000, 0.000000000000000000, 0.000000000000000000 ) ) ;
#669 = AXIS2_PLACEMENT_3D ( 'NONE', #6757, #1749, #3818 ) ;
#670 = EDGE_LOOP ( 'NONE', ( #4477, #1175, #12160, #8347 ) ) ;
#671 = FACE_BOUND ( 'NONE', #6645, .T. ) ;
#672 = APPLICATION_CONTEXT ( 'automotive_design' ) ;
#673 = CARTESIAN_POINT ( 'NONE',  ( 4.999999999999999112, -22.83261415639492142, -14.41081992069334028 ) ) ;
#674 = ORIENTED_EDGE ( 'NONE', *, *, #7139, .T. ) ;
#675 = DIRECTION ( 'NONE',  ( 0.000000000000000000, 0.000000000000000000, 1.000000000000000000 ) ) ;
#676 = ADVANCED_FACE ( 'NONE', ( #1939 ), #5688, .T. ) ;
#677 = CIRCLE ( 'NONE', #7465, 5.000000000000004441 ) ;
#678 = SHAPE_REPRESENTATION ( 'hub', ( #6056 ), #8623 ) ;
#679 = ORIENTED_EDGE ( 'NONE', *, *, #2867, .F. ) ;
#680 = DIRECTION ( 'NONE',  ( 0.000000000000000000, 0.000000000000000000, -1.000000000000000000 ) ) ;
#681 = VERTEX_POINT ( 'NONE', #9507 ) ;
#682 = CARTESIAN_POINT ( 'NONE',  ( 36.00000000000000711, 34.64101615137756340, -19.99999999999998934 ) ) ;
#683 = AXIS2_PLACEMENT_3D ( 'NONE', #333, #4146, #1473 ) ;
#684 = ORIENTED_EDGE ( 'NONE', *, *, #6242, .F. ) ;
#685 = DIRECTION ( 'NONE',  ( -1.000000000000000000, -0.000000000000000000, -0.000000000000000000 ) ) ;
#686 = CYLINDRICAL_SURFACE ( 'NONE', #10173, 0.7500000000000000000 ) ;
#687 = EDGE_CURVE ( 'NONE', #7798, #6404, #4400, .T. ) ;
#688 = DIRECTION ( 'NONE',  ( 0.000000000000000000, -0.000000000000000000, 1.000000000000000000 ) ) ;
#689 = PLANE ( 'NONE',  #1651 ) ;
#690 = ORIENTED_EDGE ( 'NONE', *, *, #8695, .T. ) ;
#691 = ORIENTED_EDGE ( 'NONE', *, *, #7322, .T. ) ;
#692 = CARTESIAN_POINT ( 'NONE',  ( 0.000000000000000000, 5.950465759859149273, -20.13931372320382351 ) ) ;
#693 = SURFACE_STYLE_FILL_AREA ( #10937 ) ;
#694 = DIRECTION ( 'NONE',  ( -1.000000000000000000, -0.000000000000000000, 0.000000000000000000 ) ) ;
#695 = ORIENTED_EDGE ( 'NONE', *, *, #8848, .T. ) ;
#696 = LINE ( 'NONE', #8326, #6294 ) ;
#697 = ORIENTED_EDGE ( 'NONE', *, *, #12266, .F. ) ;
#698 = DIRECTION ( 'NONE',  ( 1.000000000000000000, 0.000000000000000000, 0.000000000000000000 ) ) ;
#699 = CIRCLE ( 'NONE', #3309, 7.000000000000006217 ) ;
#700 = DIRECTION ( 'NONE',  ( -1.000000000000000000, 0.000000000000000000, -0.000000000000000000 ) ) ;
#701 = CYLINDRICAL_SURFACE ( 'NONE', #1923, 2.396904916527700102 ) ;
#702 = VERTEX_POINT ( 'NONE', #9699 ) ;
#703 = DIRECTION ( 'NONE',  ( -1.000000000000000000, -0.000000000000000000, 0.000000000000000000 ) ) ;
#704 = LINE ( 'NONE', #8215, #4042 ) ;
#705 = ORIENTED_EDGE ( 'NONE', *, *, #5884, .T. ) ;
#706 = CARTESIAN_POINT ( 'NONE',  ( 4.999999999999999112, 0.000000000000000000, 0.000000000000000000 ) ) ;
#707 = AXIS2_PLACEMENT_3D ( 'NONE', #6696, #7558, #9442 ) ;
#708 = CARTESIAN_POINT ( 'NONE',  ( 1.600000000000000089, 0.000000000000000000, 7.000000000000000000 ) ) ;
#709 = VERTEX_POINT ( 'NONE', #9052 ) ;
#710 = VERTEX_POINT ( 'NONE', #2878 ) ;
#711 = EDGE_CURVE ( 'NONE', #8590, #2532, #9562, .T. ) ;
#712 = EDGE_CURVE ( 'NONE', #1430, #4680, #8632, .T. ) ;
#713 = SURFACE_STYLE_USAGE ( .BOTH. , #6225 ) ;
#714 = CARTESIAN_POINT ( 'NONE',  ( 0.000000000000000000, 5.950465759858868608, 20.13931372320390523 ) ) ;
#715 = DIRECTION ( 'NONE',  ( 1.000000000000000000, 0.000000000000000000, 0.000000000000000000 ) ) ;
#716 = DIRECTION ( 'NONE',  ( -1.000000000000000000, -0.000000000000000000, -0.000000000000000000 ) ) ;
#717 = FACE_OUTER_BOUND ( 'NONE', #8562, .T. ) ;
#718 = VERTEX_POINT ( 'NONE', #9000 ) ;
#719 = DIRECTION ( 'NONE',  ( -1.000000000000000000, 0.000000000000000000, -0.000000000000000000 ) ) ;
#720 = VERTEX_POINT ( 'NONE', #5305 ) ;
#721 = CARTESIAN_POINT ( 'NONE',  ( 4.999999999999999112, -20.13931372320384128, -5.950465759859079995 ) ) ;
#722 = DIRECTION ( 'NONE',  ( -2.598194829928302921E-18, -0.5446390350150289716, 0.8386705679454229401 ) ) ;
#723 = ORIENTED_EDGE ( 'NONE', *, *, #8714, .T. ) ;
#724 = DIRECTION ( 'NONE',  ( -0.000000000000000000, 0.000000000000000000, 1.000000000000000000 ) ) ;
#725 = EDGE_CURVE ( 'NONE', #185, #9803, #1207, .T. ) ;
#726 = CARTESIAN_POINT ( 'NONE',  ( 26.00000000000000355, 0.000000000000000000, 0.000000000000000000 ) ) ;
#727 = ADVANCED_FACE ( 'NONE', ( #351 ), #5059, .F. ) ;
#728 = ADVANCED_FACE ( 'NONE', ( #419 ), #10867, .T. ) ;
#729 = ORIENTED_EDGE ( 'NONE', *, *, #1755, .F. ) ;
#730 = DIRECTION ( 'NONE',  ( 1.000000000000000000, 0.000000000000000000, 0.000000000000000000 ) ) ;
#731 = ORIENTED_EDGE ( 'NONE', *, *, #5183, .F. ) ;
#732 = CYLINDRICAL_SURFACE ( 'NONE', #1380, 7.200000000007202416 ) ;
#733 = VERTEX_POINT ( 'NONE', #6119 ) ;
#734 = DIRECTION ( 'NONE',  ( 1.000000000000000000, -0.000000000000000000, 0.000000000000000000 ) ) ;
#735 = ORIENTED_EDGE ( 'NONE', *, *, #8854, .T. ) ;
#736 = DIRECTION ( 'NONE',  ( 0.000000000000000000, 0.000000000000000000, 1.000000000000000000 ) ) ;
#737 = PRODUCT_RELATED_PRODUCT_CATEGORY ( 'part', '', ( #330 ) ) ;
#738 = FACE_OUTER_BOUND ( 'NONE', #6740, .T. ) ;
#739 = FACE_OUTER_BOUND ( 'NONE', #4011, .T. ) ;
#740 = DIRECTION ( 'NONE',  ( 0.000000000000000000, -0.4999999999999889533, -0.8660254037844451469 ) ) ;
#741 = EDGE_LOOP ( 'NONE', ( #2743, #11355 ) ) ;
#742 = ORIENTED_EDGE ( 'NONE', *, *, #4488, .F. ) ;
#743 = DIRECTION ( 'NONE',  ( -1.000000000000000000, 0.000000000000000000, 0.000000000000000000 ) ) ;
#744 = LINE ( 'NONE', #7334, #3036 ) ;
#745 = DIRECTION ( 'NONE',  ( 0.000000000000000000, 0.000000000000000000, 1.000000000000000000 ) ) ;
#746 = EDGE_CURVE ( 'NONE', #8081, #1083, #9126, .T. ) ;
#747 = ORIENTED_EDGE ( 'NONE', *, *, #7161, .T. ) ;
#748 = FACE_OUTER_BOUND ( 'NONE', #2914, .T. ) ;
#749 = EDGE_CURVE ( 'NONE', #10239, #7044, #9805, .T. ) ;
#750 = DIRECTION ( 'NONE',  ( 0.000000000000000000, 0.000000000000000000, 1.000000000000000000 ) ) ;
#751 = DIRECTION ( 'NONE',  ( 0.000000000000000000, -1.000000000000000000, 0.000000000000000000 ) ) ;
#752 = VERTEX_POINT ( 'NONE', #6992 ) ;
#753 = DIRECTION ( 'NONE',  ( 0.000000000000000000, 8.881784197001252323E-16, 1.000000000000000000 ) ) ;
#754 = DIRECTION ( 'NONE',  ( -1.000000000000000000, -0.000000000000000000, -0.000000000000000000 ) ) ;
#755 = ORIENTED_EDGE ( 'NONE', *, *, #1742, .T. ) ;
#756 = CARTESIAN_POINT ( 'NONE',  ( 65.79898987322334847, -9.445087446769608850E-17, -41.99999999999998579 ) ) ;
#757 = DIRECTION ( 'NONE',  ( 0.000000000000000000, 0.000000000000000000, 1.000000000000000000 ) ) ;
#758 = AXIS2_PLACEMENT_3D ( 'NONE', #5741, #8694, #117 ) ;
#759 = ORIENTED_EDGE ( 'NONE', *, *, #9853, .T. ) ;
#760 = CARTESIAN_POINT ( 'NONE',  ( 0.000000000000000000, -22.37914155802283034, 6.808078995945121115 ) ) ;
#761 = ORIENTED_EDGE ( 'NONE', *, *, #8385, .F. ) ;
#762 = VECTOR ( 'NONE', #7033, 1000.000000000000000 ) ;
#763 =( NAMED_UNIT ( * ) SI_UNIT ( $, .STERADIAN. ) SOLID_ANGLE_UNIT ( ) );
#764 = CIRCLE ( 'NONE', #11939, 7.200000000007202416 ) ;
#765 = CARTESIAN_POINT ( 'NONE',  ( 3.309651814758565180, -5.455921364805393026, 0.000000000000000000 ) ) ;
#766 = DIRECTION ( 'NONE',  ( 0.000000000000000000, 0.000000000000000000, 1.000000000000000000 ) ) ;
#767 = AXIS2_PLACEMENT_3D ( 'NONE', #1245, #5249, #6889 ) ;
#768 = CARTESIAN_POINT ( 'NONE',  ( 4.999999999999999112, 15.37949036966211835, 13.17168466712934105 ) ) ;
#769 = DIRECTION ( 'NONE',  ( 1.000000000000000000, 0.000000000000000000, 0.000000000000000000 ) ) ;
#770 = EDGE_LOOP ( 'NONE', ( #10849, #2920, #12300, #11443 ) ) ;
#771 = EDGE_LOOP ( 'NONE', ( #6888, #1800 ) ) ;
#772 = CARTESIAN_POINT ( 'NONE',  ( 4.999999999999999112, -19.24938187143300539, 6.283573709965241783 ) ) ;
#773 = ORIENTED_EDGE ( 'NONE', *, *, #711, .F. ) ;
#774 = DIRECTION ( 'NONE',  ( -1.000000000000000000, 0.000000000000000000, -0.000000000000000000 ) ) ;
#775 = EDGE_CURVE ( 'NONE', #5859, #1347, #8071, .T. ) ;
#776 = DIRECTION ( 'NONE',  ( 1.000000000000000000, -4.770489558936235687E-18, 6.855277276495153692E-34 ) ) ;
#777 = VERTEX_POINT ( 'NONE', #5243 ) ;
#779 = CARTESIAN_POINT ( 'NONE',  ( 4.999999999999999112, -0.4834863907626938961, 16.90755573046746107 ) ) ;
#778 = VECTOR ( 'NONE', #11528, 1000.000000000000000 ) ;
#780 = FACE_OUTER_BOUND ( 'NONE', #2241, .T. ) ;
#781 = VECTOR ( 'NONE', #6291, 1000.000000000000000 ) ;
#782 = ORIENTED_EDGE ( 'NONE', *, *, #12280, .F. ) ;
#783 = CARTESIAN_POINT ( 'NONE',  ( 4.999999999999999112, 9.168210874537823685, -18.05452603534156353 ) ) ;
#784 = CARTESIAN_POINT ( 'NONE',  ( 4.999999999999999112, 1.561154383803505796, -20.18872947935929574 ) ) ;
#785 = EDGE_CURVE ( 'NONE', #11661, #5342, #1300, .T. ) ;
#786 = ORIENTED_EDGE ( 'NONE', *, *, #9903, .T. ) ;
#787 = MECHANICAL_DESIGN_GEOMETRIC_PRESENTATION_REPRESENTATION (  '', ( #4384 ), #9194 ) ;
#788 = DIRECTION ( 'NONE',  ( 0.000000000000000000, 0.000000000000000000, 1.000000000000000000 ) ) ;
#789 = ORIENTED_EDGE ( 'NONE', *, *, #5630, .T. ) ;
#790 = EDGE_CURVE ( 'NONE', #1934, #9986, #4294, .T. ) ;
#791 = ADVANCED_FACE ( 'NONE', ( #302 ), #11781, .T. ) ;
#792 = DIRECTION ( 'NONE',  ( -1.000000000000000000, -0.000000000000000000, -0.000000000000000000 ) ) ;
#793 = EDGE_LOOP ( 'NONE', ( #3295, #4866 ) ) ;
#794 = FACE_OUTER_BOUND ( 'NONE', #9487, .T. ) ;
#795 = PRESENTATION_LAYER_ASSIGNMENT (  '', '', ( #3009 ) ) ;
#796 = AXIS2_PLACEMENT_3D ( 'NONE', #6249, #10798, #2238 ) ;
#797 = DIRECTION ( 'NONE',  ( 0.000000000000000000, 0.000000000000000000, 1.000000000000000000 ) ) ;
#798 = DIRECTION ( 'NONE',  ( 1.000000000000000000, 0.000000000000000000, 0.000000000000000000 ) ) ;
#799 = CARTESIAN_POINT ( 'NONE',  ( 42.00000000000000000, 6.799999999999998046, 1.500000000000000000 ) ) ;
#800 = AXIS2_PLACEMENT_3D ( 'NONE', #10645, #2078, #1132 ) ;
#801 = EDGE_LOOP ( 'NONE', ( #10590, #9547, #9131, #11331 ) ) ;
#802 = EDGE_LOOP ( 'NONE', ( #5664, #1167, #12118, #8865 ) ) ;
#803 = DIRECTION ( 'NONE',  ( -1.000000000000000000, 0.000000000000000000, 0.000000000000000000 ) ) ;
#804 = EDGE_CURVE ( 'NONE', #2076, #10859, #397, .T. ) ;
#805 = VECTOR ( 'NONE', #2259, 1000.000000000000000 ) ;
#806 = CARTESIAN_POINT ( 'NONE',  ( 4.999999999999999112, 11.14352537685174660, 19.60720892790256897 ) ) ;
#807 = EDGE_CURVE ( 'NONE', #5230, #2486, #7399, .T. ) ;
#808 = AXIS2_PLACEMENT_3D ( 'NONE', #8681, #7740, #7549 ) ;
#809 = EDGE_CURVE ( 'NONE', #5401, #8263, #6062, .T. ) ;
#810 = CARTESIAN_POINT ( 'NONE',  ( 4.999999999999999112, -1.561154383803080581, -20.18872947935932771 ) ) ;
#811 = VERTEX_POINT ( 'NONE', #6939 ) ;
#812 = CARTESIAN_POINT ( 'NONE',  ( 36.00000000000000711, 1.456773409934505593E-31, -36.99999999999998579 ) ) ;
#813 = AXIS2_PLACEMENT_3D ( 'NONE', #11633, #7898, #11689 ) ;
#814 = CIRCLE ( 'NONE', #11987, 0.7499999999999997780 ) ;
#815 = AXIS2_PLACEMENT_3D ( 'NONE', #1986, #6874, #10541 ) ;
#816 = VECTOR ( 'NONE', #12136, 1000.000000000000000 ) ;
#817 = VECTOR ( 'NONE', #8993, 1000.000000000000000 ) ;
#818 = DIRECTION ( 'NONE',  ( -1.000000000000000000, -0.000000000000000000, 0.000000000000000000 ) ) ;
#819 = CARTESIAN_POINT ( 'NONE',  ( 1.095413108702814053, 4.828698707966718301E-16, 3.885863436426969297 ) ) ;
#820 = ADVANCED_FACE ( 'NONE', ( #1492 ), #6175, .T. ) ;
#821 = ORIENTED_EDGE ( 'NONE', *, *, #2283, .F. ) ;
#822 = EDGE_CURVE ( 'NONE', #4760, #6667, #10739, .T. ) ;
#823 = DIRECTION ( 'NONE',  ( 0.000000000000000000, 1.000000000000000000, 3.491481338843133355E-15 ) ) ;
#824 = CARTESIAN_POINT ( 'NONE',  ( 43.00000000000000000, -2.824006678639516377, 3.881363971466655904 ) ) ;
#825 = VERTEX_POINT ( 'NONE', #483 ) ;
#826 = DIRECTION ( 'NONE',  ( 0.000000000000000000, 0.000000000000000000, 1.000000000000000000 ) ) ;
#827 = CARTESIAN_POINT ( 'NONE',  ( -20.00000000000000000, 44.00000000000001421, -12.50000000000000000 ) ) ;
#828 = VECTOR ( 'NONE', #8616, 1000.000000000000000 ) ;
#829 = EDGE_LOOP ( 'NONE', ( #5890, #10432, #3205, #5681, #3589, #1932, #7496, #8486 ) ) ;
#830 = CARTESIAN_POINT ( 'NONE',  ( 0.000000000000000000, -16.90755573046745752, -0.4834863907627537372 ) ) ;
#831 = CIRCLE ( 'NONE', #11809, 9.600000000009600853 ) ;
#832 = AXIS2_PLACEMENT_3D ( 'NONE', #4718, #6732, #8723 ) ;
#833 = EDGE_LOOP ( 'NONE', ( #9307, #5030, #4044, #11673 ) ) ;
#834 = CIRCLE ( 'NONE', #4220, 20.24900000002024569 ) ;
#835 = CARTESIAN_POINT ( 'NONE',  ( 42.00000000000000000, 0.000000000000000000, 0.000000000000000000 ) ) ;
#836 = CIRCLE ( 'NONE', #7636, 21.00000000002100009 ) ;
#837 = VECTOR ( 'NONE', #8894, 1000.000000000000000 ) ;
#838 = CARTESIAN_POINT ( 'NONE',  ( 4.999999999999999112, 0.000000000000000000, 0.000000000000000000 ) ) ;
#839 = DIRECTION ( 'NONE',  ( 1.000000000000000000, -4.770489558936236458E-18, 6.855277276495154548E-34 ) ) ;
#840 = ADVANCED_FACE ( 'NONE', ( #2297 ), #10980, .F. ) ;
#841 = AXIS2_PLACEMENT_3D ( 'NONE', #8106, #3340, #7915 ) ;
#842 = DIRECTION ( 'NONE',  ( 1.000000000000000000, -0.000000000000000000, -0.000000000000000000 ) ) ;
#843 = LINE ( 'NONE', #5480, #11789 ) ;
#844 = ORIENTED_EDGE ( 'NONE', *, *, #6702, .F. ) ;
#845 = ORIENTED_EDGE ( 'NONE', *, *, #3771, .T. ) ;
#846 = CARTESIAN_POINT ( 'NONE',  ( 37.00000000000000711, -2.172883482918394282, 4.280020720704565740 ) ) ;
#847 = EDGE_LOOP ( 'NONE', ( #6303, #2605, #4800, #9954 ) ) ;
#848 = DIRECTION ( 'NONE',  ( -1.000000000000000000, 0.000000000000000000, 0.000000000000000000 ) ) ;
#849 = DIRECTION ( 'NONE',  ( 0.000000000000000000, 0.6828850436591805684, 0.7305258497456464939 ) ) ;
#850 = EDGE_LOOP ( 'NONE', ( #7886, #4697, #10680, #9743 ) ) ;
#851 = CARTESIAN_POINT ( 'NONE',  ( -0.1481481481481481122, -4.797713218419819903, -1.000000000000000000 ) ) ;
#852 = VECTOR ( 'NONE', #909, 1000.000000000000000 ) ;
#853 = AXIS2_PLACEMENT_3D ( 'NONE', #10883, #7084, #7954 ) ;
#854 = DIRECTION ( 'NONE',  ( -1.000000000000000000, 0.000000000000000000, 0.000000000000000000 ) ) ;
#855 = ORIENTED_EDGE ( 'NONE', *, *, #7367, .F. ) ;
#856 = ORIENTED_EDGE ( 'NONE', *, *, #10508, .F. ) ;
#857 = DIRECTION ( 'NONE',  ( 1.000000000000000000, 0.000000000000000000, 0.000000000000000000 ) ) ;
#858 = LINE ( 'NONE', #11064, #11986 ) ;
#859 = DIRECTION ( 'NONE',  ( -1.000000000000000000, -0.000000000000000000, 0.000000000000000000 ) ) ;
#860 = EDGE_LOOP ( 'NONE', ( #11769, #4561 ) ) ;
#861 = AXIS2_PLACEMENT_3D ( 'NONE', #6268, #3378, #6379 ) ;
#862 = DIRECTION ( 'NONE',  ( -1.000000000000000000, 0.000000000000000000, 0.000000000000000000 ) ) ;
#863 = VERTEX_POINT ( 'NONE', #1425 ) ;
#864 = FILL_AREA_STYLE_COLOUR ( '', #1845 ) ;
#865 = CARTESIAN_POINT ( 'NONE',  ( 1.400000000000001910, 0.000000000000000000, 0.000000000000000000 ) ) ;
#866 = VERTEX_POINT ( 'NONE', #8127 ) ;
#867 = FACE_OUTER_BOUND ( 'NONE', #2412, .T. ) ;
#868 = ADVANCED_FACE ( 'NONE', ( #4542 ), #9206, .T. ) ;
#869 = AXIS2_PLACEMENT_3D ( 'NONE', #8640, #3886, #11494 ) ;
#870 = DIRECTION ( 'NONE',  ( 0.000000000000000000, 0.000000000000000000, -1.000000000000000000 ) ) ;
#871 = EDGE_CURVE ( 'NONE', #3139, #7019, #10116, .T. ) ;
#872 = DIRECTION ( 'NONE',  ( 1.000000000000000000, 0.000000000000000000, 0.000000000000000000 ) ) ;
#873 = CARTESIAN_POINT ( 'NONE',  ( -20.00000000000000000, 44.00000000000001421, -12.50000000000000000 ) ) ;
#874 = ORIENTED_EDGE ( 'NONE', *, *, #4487, .F. ) ;
#875 = ORIENTED_EDGE ( 'NONE', *, *, #5689, .T. ) ;
#876 = DIRECTION ( 'NONE',  ( -1.000000000000000000, 0.000000000000000000, 0.000000000000000000 ) ) ;
#877 = AXIS2_PLACEMENT_3D ( 'NONE', #8794, #2853, #1099 ) ;
#878 = SURFACE_STYLE_USAGE ( .BOTH. , #7454 ) ;
#879 = LINE ( 'NONE', #8202, #4628 ) ;
#880 = LINE ( 'NONE', #2008, #11470 ) ;
#881 = EDGE_LOOP ( 'NONE', ( #8333, #12231, #5450, #6422 ) ) ;
#882 = LINE ( 'NONE', #1075, #4787 ) ;
#883 = EDGE_CURVE ( 'NONE', #6238, #3985, #11291, .T. ) ;
#884 = EDGE_CURVE ( 'NONE', #5539, #7662, #4798, .T. ) ;
#885 = VECTOR ( 'NONE', #86, 1000.000000000000000 ) ;
#886 = EDGE_CURVE ( 'NONE', #1449, #11926, #6396, .T. ) ;
#887 = EDGE_CURVE ( 'NONE', #4391, #5044, #9592, .T. ) ;
#888 = DIRECTION ( 'NONE',  ( -1.000000000000000000, -0.000000000000000000, 0.000000000000000000 ) ) ;
#889 = CARTESIAN_POINT ( 'NONE',  ( -5.686050877451574337, -5.768780236673276995, -1.000000000000000000 ) ) ;
#890 = CARTESIAN_POINT ( 'NONE',  ( 4.999999999999999112, -14.41081992069325679, 22.83261415639497471 ) ) ;
#891 = LINE ( 'NONE', #5758, #6852 ) ;
#892 = EDGE_LOOP ( 'NONE', ( #2724, #5114, #7799, #6342 ) ) ;
#893 = DIRECTION ( 'NONE',  ( 0.000000000000000000, 0.000000000000000000, 1.000000000000000000 ) ) ;
#894 = DIRECTION ( 'NONE',  ( -1.000000000000000000, 0.000000000000000000, 0.000000000000000000 ) ) ;
#895 = ORIENTED_EDGE ( 'NONE', *, *, #9149, .F. ) ;
#896 = LINE ( 'NONE', #2903, #4889 ) ;
#897 = UNCERTAINTY_MEASURE_WITH_UNIT (LENGTH_MEASURE( 1.000000000000000082E-05 ), #10067, 'distance_accuracy_value', 'NONE');
#898 = CIRCLE ( 'NONE', #10278, 9.600000000009600853 ) ;
#899 = EDGE_LOOP ( 'NONE', ( #6133, #4541, #600, #8975 ) ) ;
#900 = CARTESIAN_POINT ( 'NONE',  ( 2.500000000000000000, -1.178949249685213863, 2.042000000000002924 ) ) ;
#901 = APPLICATION_CONTEXT ( 'automotive_design' ) ;
#902 = CARTESIAN_POINT ( 'NONE',  ( 2.499999999999999556, 22.05152472667129970, 15.57980286237480172 ) ) ;
#903 = DIRECTION ( 'NONE',  ( 1.000000000000000000, -0.000000000000000000, -0.000000000000000000 ) ) ;
#904 = AXIS2_PLACEMENT_3D ( 'NONE', #4247, #10925, #2491 ) ;
#905 = DIRECTION ( 'NONE',  ( -1.000000000000000000, -0.000000000000000000, -0.000000000000000000 ) ) ;
#906 = FACE_OUTER_BOUND ( 'NONE', #10491, .T. ) ;
#907 = ORIENTED_EDGE ( 'NONE', *, *, #12203, .T. ) ;
#908 = VERTEX_POINT ( 'NONE', #5430 ) ;
#909 = DIRECTION ( 'NONE',  ( -1.000000000000000000, 0.000000000000000000, 0.000000000000000000 ) ) ;
#910 = ORIENTED_EDGE ( 'NONE', *, *, #7161, .F. ) ;
#911 = SURFACE_SIDE_STYLE ('',( #8729 ) ) ;
#912 = EDGE_LOOP ( 'NONE', ( #4953, #8523 ) ) ;
#913 = CYLINDRICAL_SURFACE ( 'NONE', #418, 2.000000000000000000 ) ;
#914 = EDGE_CURVE ( 'NONE', #4485, #1003, #11235, .T. ) ;
#915 = FACE_OUTER_BOUND ( 'NONE', #11711, .T. ) ;
#916 = EDGE_CURVE ( 'NONE', #5149, #331, #3822, .T. ) ;
#917 = ORIENTED_EDGE ( 'NONE', *, *, #305, .F. ) ;
#918 = ORIENTED_EDGE ( 'NONE', *, *, #7157, .T. ) ;
#919 = CARTESIAN_POINT ( 'NONE',  ( 3.309651814758565180, -5.455921364805393026, -1.000000000000000000 ) ) ;
#920 = LINE ( 'NONE', #10484, #4416 ) ;
#921 = DIRECTION ( 'NONE',  ( 1.000000000000000000, 0.000000000000000000, 0.000000000000000000 ) ) ;
#922 = VERTEX_POINT ( 'NONE', #4486 ) ;
#923 = DIRECTION ( 'NONE',  ( -1.000000000000000000, 0.000000000000000000, 0.000000000000000000 ) ) ;
#924 = ORIENTED_EDGE ( 'NONE', *, *, #6368, .T. ) ;
#925 = FILL_AREA_STYLE_COLOUR ( '', #9637 ) ;
#926 = ORIENTED_EDGE ( 'NONE', *, *, #1803, .F. ) ;
#927 = DIRECTION ( 'NONE',  ( 0.000000000000000000, 0.000000000000000000, -1.000000000000000000 ) ) ;
#928 = ORIENTED_EDGE ( 'NONE', *, *, #2879, .F. ) ;
#929 = LINE ( 'NONE', #8563, #1357 ) ;
#930 = CARTESIAN_POINT ( 'NONE',  ( 0.000000000000000000, 0.000000000000000000, 0.000000000000000000 ) ) ;
#931 = CARTESIAN_POINT ( 'NONE',  ( 0.000000000000000000, -14.14998813191268390, -1.676853263448035536 ) ) ;
#932 = CARTESIAN_POINT ( 'NONE',  ( 0.000000000000000000, -14.46592441914954286, -15.22291137398937089 ) ) ;
#933 = EDGE_LOOP ( 'NONE', ( #2044, #3069, #11821, #10973 ) ) ;
#934 = ORIENTED_EDGE ( 'NONE', *, *, #8998, .T. ) ;
#935 = DIRECTION ( 'NONE',  ( 0.000000000000000000, 0.000000000000000000, -1.000000000000000000 ) ) ;
#936 =( NAMED_UNIT ( * ) SI_UNIT ( $, .STERADIAN. ) SOLID_ANGLE_UNIT ( ) );
#937 = CARTESIAN_POINT ( 'NONE',  ( 4.999999999999999112, -17.79862902732275032, 13.85025647830051021 ) ) ;
#938 = DIRECTION ( 'NONE',  ( 1.000000000000000000, 1.734723475976807094E-16, 0.000000000000000000 ) ) ;
#939 = EDGE_CURVE ( 'NONE', #1873, #5296, #2217, .T. ) ;
#940 = ORIENTED_EDGE ( 'NONE', *, *, #499, .T. ) ;
#941 = CARTESIAN_POINT ( 'NONE',  ( 0.1481481481481481122, -4.797713218419819903, 0.000000000000000000 ) ) ;
#942 = DIRECTION ( 'NONE',  ( 0.000000000000000000, 0.000000000000000000, 1.000000000000000000 ) ) ;
#943 = DIRECTION ( 'NONE',  ( -1.000000000000000000, -0.000000000000000000, -0.000000000000000000 ) ) ;
#944 = FACE_BOUND ( 'NONE', #8542, .T. ) ;
#945 = ORIENTED_EDGE ( 'NONE', *, *, #12203, .F. ) ;
#946 = EDGE_CURVE ( 'NONE', #2151, #1926, #10200, .T. ) ;
#947 = CARTESIAN_POINT ( 'NONE',  ( 4.999999999999999112, -22.37914155802283034, 6.808078995945121115 ) ) ;
#948 = FACE_OUTER_BOUND ( 'NONE', #120, .T. ) ;
#949 = ORIENTED_EDGE ( 'NONE', *, *, #2650, .T. ) ;
#950 = CARTESIAN_POINT ( 'NONE',  ( 1.000000000000000000, -0.5999999999999994227, -4.000000000000000000 ) ) ;
#951 = ADVANCED_FACE ( 'NONE', ( #2674 ), #3495, .T. ) ;
#952 = ORIENTED_EDGE ( 'NONE', *, *, #7096, .F. ) ;
#953 = EDGE_CURVE ( 'NONE', #8701, #7793, #8813, .T. ) ;
#954 = CARTESIAN_POINT ( 'NONE',  ( -2.000000000000000000, -6.429618962271402616, -1.000000000000000000 ) ) ;
#955 = CARTESIAN_POINT ( 'NONE',  ( 45.00000000000000000, 0.000000000000000000, 0.000000000000000000 ) ) ;
#956 = CARTESIAN_POINT ( 'NONE',  ( 37.00000000000000711, -4.104405154062230115E-16, -2.224720805914714718E-17 ) ) ;
#957 = DIRECTION ( 'NONE',  ( 1.000000000000000000, 0.000000000000000000, 0.000000000000000000 ) ) ;
#958 = LINE ( 'NONE', #4848, #8432 ) ;
#959 = ORIENTED_EDGE ( 'NONE', *, *, #12102, .F. ) ;
#960 = ORIENTED_EDGE ( 'NONE', *, *, #7258, .T. ) ;
#961 = SURFACE_SIDE_STYLE ('',( #5858 ) ) ;
#962 = AXIS2_PLACEMENT_3D ( 'NONE', #956, #4845, #9481 ) ;
#963 = ORIENTED_EDGE ( 'NONE', *, *, #1656, .T. ) ;
#964 = DIRECTION ( 'NONE',  ( 0.000000000000000000, 0.000000000000000000, 1.000000000000000000 ) ) ;
#965 = EDGE_CURVE ( 'NONE', #9862, #8991, #4609, .T. ) ;
#966 =( NAMED_UNIT ( * ) PLANE_ANGLE_UNIT ( ) SI_UNIT ( $, .RADIAN. ) );
#967 = ORIENTED_EDGE ( 'NONE', *, *, #11197, .F. ) ;
#968 = EDGE_CURVE ( 'NONE', #2318, #8881, #10351, .T. ) ;
#969 = CARTESIAN_POINT ( 'NONE',  ( 29.00000000000000000, 0.000000000000000000, -41.99999999999999289 ) ) ;
#970 = AXIS2_PLACEMENT_3D ( 'NONE', #8936, #4115, #7935 ) ;
#971 = VECTOR ( 'NONE', #6375, 1000.000000000000000 ) ;
#972 = VERTEX_POINT ( 'NONE', #6546 ) ;
#973 = ORIENTED_EDGE ( 'NONE', *, *, #8939, .F. ) ;
#974 = DIRECTION ( 'NONE',  ( 1.000000000000000000, -0.000000000000000000, -0.000000000000000000 ) ) ;
#975 = CARTESIAN_POINT ( 'NONE',  ( 4.999999999999997335, 6.123233995736766282E-16, -5.000000000000000000 ) ) ;
#976 = LINE ( 'NONE', #5872, #2034 ) ;
#977 = CARTESIAN_POINT ( 'NONE',  ( 33.00000000000000000, 0.000000000000000000, 0.000000000000000000 ) ) ;
#978 = VERTEX_POINT ( 'NONE', #783 ) ;
#979 = EDGE_CURVE ( 'NONE', #3276, #5514, #4817, .T. ) ;
#980 = EDGE_CURVE ( 'NONE', #1358, #1101, #4200, .T. ) ;
#981 = PLANE ( 'NONE',  #380 ) ;
#982 = CIRCLE ( 'NONE', #4170, 9.600000000009599077 ) ;
#983 = ORIENTED_EDGE ( 'NONE', *, *, #11550, .F. ) ;
#984 = VECTOR ( 'NONE', #605, 999.9999999999998863 ) ;
#985 =( NAMED_UNIT ( * ) SI_UNIT ( $, .STERADIAN. ) SOLID_ANGLE_UNIT ( ) );
#986 = ORIENTED_EDGE ( 'NONE', *, *, #11375, .F. ) ;
#987 = AXIS2_PLACEMENT_3D ( 'NONE', #10904, #3051, #6923 ) ;
#988 = PLANE ( 'NONE',  #3703 ) ;
#989 = EDGE_LOOP ( 'NONE', ( #76, #684, #3610, #12217 ) ) ;
#990 = FACE_OUTER_BOUND ( 'NONE', #7425, .T. ) ;
#991 = CIRCLE ( 'NONE', #11951, 6.000000000000005329 ) ;
#992 = VECTOR ( 'NONE', #7075, 1000.000000000000000 ) ;
#993 = DIRECTION ( 'NONE',  ( 0.000000000000000000, -0.5000000000000011102, -0.8660254037844379305 ) ) ;
#994 = AXIS2_PLACEMENT_3D ( 'NONE', #5555, #4555, #9267 ) ;
#995 = CARTESIAN_POINT ( 'NONE',  ( 0.8601259673543576456, -0.6000000000000000888, 3.802963942891089300 ) ) ;
#996 = CARTESIAN_POINT ( 'NONE',  ( 4.999999999999999112, 20.13931372320388391, 5.950465759858937886 ) ) ;
#997 = VERTEX_POINT ( 'NONE', #8434 ) ;
#998 = DIRECTION ( 'NONE',  ( -0.000000000000000000, -0.000000000000000000, -1.000000000000000000 ) ) ;
#999 = SURFACE_STYLE_FILL_AREA ( #8572 ) ;
#1000 = CARTESIAN_POINT ( 'NONE',  ( 36.00000000000000711, 0.000000000000000000, 0.000000000000000000 ) ) ;
#1001 = AXIS2_PLACEMENT_3D ( 'NONE', #7684, #2154, #6925 ) ;
#1002 = DIRECTION ( 'NONE',  ( 0.000000000000000000, 0.000000000000000000, -1.000000000000000000 ) ) ;
#1003 = VERTEX_POINT ( 'NONE', #9431 ) ;
#1004 = DIRECTION ( 'NONE',  ( -1.000000000000000000, 0.000000000000000000, -0.000000000000000000 ) ) ;
#1005 = CIRCLE ( 'NONE', #9001, 4.000000000000000000 ) ;
#1006 = AXIS2_PLACEMENT_3D ( 'NONE', #1909, #9667, #145 ) ;
#1007 = LINE ( 'NONE', #5641, #2212 ) ;
#1008 = DIRECTION ( 'NONE',  ( 0.000000000000000000, 0.000000000000000000, -1.000000000000000000 ) ) ;
#1009 = AXIS2_PLACEMENT_3D ( 'NONE', #919, #6687, #8735 ) ;
#1010 = CARTESIAN_POINT ( 'NONE',  ( 0.1920286436967153787, 0.000000000000000000, 0.000000000000000000 ) ) ;
#1011 = DIRECTION ( 'NONE',  ( -0.000000000000000000, 0.000000000000000000, -1.000000000000000000 ) ) ;
#1012 = ORIENTED_EDGE ( 'NONE', *, *, #1063, .F. ) ;
#1013 = CARTESIAN_POINT ( 'NONE',  ( 4.999999999999999112, -14.88411597386734897, 8.035066368449154339 ) ) ;
#1014 = DIRECTION ( 'NONE',  ( 0.000000000000000000, 0.000000000000000000, 1.000000000000000000 ) ) ;
#1015 = ORIENTED_EDGE ( 'NONE', *, *, #10828, .F. ) ;
#1016 = LINE ( 'NONE', #10518, #4484 ) ;
#1017 = UNCERTAINTY_MEASURE_WITH_UNIT (LENGTH_MEASURE( 1.000000000000000082E-05 ), #6880, 'distance_accuracy_value', 'NONE');
#1018 = ORIENTED_EDGE ( 'NONE', *, *, #2208, .F. ) ;
#1019 = AXIS2_PLACEMENT_3D ( 'NONE', #11811, #1311, #7951 ) ;
#1020 = CIRCLE ( 'NONE', #2215, 9.600000000009599077 ) ;
#1021 = AXIS2_PLACEMENT_3D ( 'NONE', #9496, #4732, #8552 ) ;
#1022 = AXIS2_PLACEMENT_3D ( 'NONE', #5166, #4230, #8124 ) ;
#1023 = EDGE_CURVE ( 'NONE', #3084, #9327, #218, .T. ) ;
#1024 = SURFACE_SIDE_STYLE ('',( #2957 ) ) ;
#1025 = CYLINDRICAL_SURFACE ( 'NONE', #6817, 5.999999999999999112 ) ;
#1026 = DIRECTION ( 'NONE',  ( -0.000000000000000000, -0.000000000000000000, -1.000000000000000000 ) ) ;
#1027 = EDGE_CURVE ( 'NONE', #2572, #1109, #3415, .T. ) ;
#1028 = STYLED_ITEM ( 'NONE', ( #3500 ), #12103 ) ;
#1029 = CARTESIAN_POINT ( 'NONE',  ( 4.999999999999999112, 14.14998813191269633, -1.676853263447935394 ) ) ;
#1030 = CARTESIAN_POINT ( 'NONE',  ( 4.999999999999999112, 0.000000000000000000, 0.000000000000000000 ) ) ;
#1031 = CIRCLE ( 'NONE', #9223, 5.000000000000000000 ) ;
#1032 = VERTEX_POINT ( 'NONE', #6872 ) ;
#1033 = ORIENTED_EDGE ( 'NONE', *, *, #285, .T. ) ;
#1034 = CIRCLE ( 'NONE', #2618, 9.600000000009602630 ) ;
#1035 = VECTOR ( 'NONE', #1350, 1000.000000000000000 ) ;
#1036 = ORIENTED_EDGE ( 'NONE', *, *, #10914, .T. ) ;
#1037 = DIRECTION ( 'NONE',  ( -1.000000000000000000, 0.000000000000000000, 0.000000000000000000 ) ) ;
#1038 = ITEM_DEFINED_TRANSFORMATION ( 'NONE', 'NONE', #8855,  #6056 ) ;
#1039 = VERTEX_POINT ( 'NONE', #975 ) ;
#1040 = AXIS2_PLACEMENT_3D ( 'NONE', #277, #8722, #1092 ) ;
#1041 = VECTOR ( 'NONE', #11748, 1000.000000000000000 ) ;
#1042 = EDGE_CURVE ( 'NONE', #3494, #6198, #7409, .T. ) ;
#1043 = ORIENTED_EDGE ( 'NONE', *, *, #2786, .F. ) ;
#1044 = ORIENTED_EDGE ( 'NONE', *, *, #4471, .F. ) ;
#1045 = DIRECTION ( 'NONE',  ( 0.000000000000000000, 0.000000000000000000, 1.000000000000000000 ) ) ;
#1046 = CARTESIAN_POINT ( 'NONE',  ( 20.00000000000000000, 3.061616997868383043E-15, 25.00000000000000000 ) ) ;
#1047 = ADVANCED_FACE ( 'NONE', ( #3054 ), #9013, .T. ) ;
#1048 = ADVANCED_FACE ( 'NONE', ( #1157 ), #11418, .T. ) ;
#1049 = DIRECTION ( 'NONE',  ( 0.000000000000000000, 0.000000000000000000, -1.000000000000000000 ) ) ;
#1051 = EDGE_CURVE ( 'NONE', #9332, #5880, #9739, .T. ) ;
#1050 = DIRECTION ( 'NONE',  ( 0.000000000000000000, 0.8660254037844363761, 0.5000000000000041078 ) ) ;
#1052 = ORIENTED_EDGE ( 'NONE', *, *, #498, .T. ) ;
#1054 = DIRECTION ( 'NONE',  ( 1.000000000000000000, 0.000000000000000000, 0.000000000000000000 ) ) ;
#1053 = COLOUR_RGB ( '',1.000000000000000000, 0.9490196078431372140, 0.9098039215686274384 ) ;
#1055 = CIRCLE ( 'NONE', #10045, 9.600000000009600853 ) ;
#1056 = ORIENTED_EDGE ( 'NONE', *, *, #5802, .T. ) ;
#1057 = AXIS2_PLACEMENT_3D ( 'NONE', #11802, #4068, #4995 ) ;
#1058 = VECTOR ( 'NONE', #3273, 1000.000000000000000 ) ;
#1059 = ORIENTED_EDGE ( 'NONE', *, *, #9916, .T. ) ;
#1060 = DIRECTION ( 'NONE',  ( -1.000000000000000000, 0.000000000000000000, 0.000000000000000000 ) ) ;
#1061 = EDGE_LOOP ( 'NONE', ( #11023, #10557 ) ) ;
#1062 = DIRECTION ( 'NONE',  ( -1.000000000000000000, 0.000000000000000000, 0.000000000000000000 ) ) ;
#1063 = EDGE_CURVE ( 'NONE', #6538, #7124, #2051, .T. ) ;
#1064 = AXIS2_PLACEMENT_3D ( 'NONE', #11381, #6768, #9579 ) ;
#1065 = DIRECTION ( 'NONE',  ( 0.000000000000000000, 0.000000000000000000, 1.000000000000000000 ) ) ;
#1066 = VERTEX_POINT ( 'NONE', #3977 ) ;
#1067 = CYLINDRICAL_SURFACE ( 'NONE', #4355, 9.600000000009600853 ) ;
#1068 = DIRECTION ( 'NONE',  ( -1.000000000000000000, 0.000000000000000000, 0.000000000000000000 ) ) ;
#1069 = VERTEX_POINT ( 'NONE', #12286 ) ;
#1070 = CARTESIAN_POINT ( 'NONE',  ( 24.00000000000000000, 0.000000000000000000, -48.00000000000000000 ) ) ;
#1071 = DIRECTION ( 'NONE',  ( 0.000000000000000000, 0.000000000000000000, 1.000000000000000000 ) ) ;
#1072 = LINE ( 'NONE', #9514, #12068 ) ;
#1073 = VECTOR ( 'NONE', #6944, 1000.000000000000000 ) ;
#1074 = EDGE_LOOP ( 'NONE', ( #9162, #6774, #5449, #10361 ) ) ;
#1075 = CARTESIAN_POINT ( 'NONE',  ( -20.63749999999999574, 0.000000000000000000, -7.500000000000000000 ) ) ;
#1076 = EDGE_CURVE ( 'NONE', #3524, #10474, #105, .T. ) ;
#1077 = ADVANCED_FACE ( 'NONE', ( #3921 ), #10606, .T. ) ;
#1078 = DIRECTION ( 'NONE',  ( 1.000000000000000000, 0.000000000000000000, 0.000000000000000000 ) ) ;
#1079 = DIRECTION ( 'NONE',  ( -1.000000000000000000, 0.000000000000000000, -0.000000000000000000 ) ) ;
#1080 = SHAPE_REPRESENTATION ( 'spur gear_iso_ISO - Spur gear 3M 12T 20PA 5FW ---S12A75H50L10.0S1', ( #6056 ), #6434 ) ;
#1081 = DIRECTION ( 'NONE',  ( 0.000000000000000000, 0.000000000000000000, 1.000000000000000000 ) ) ;
#1082 = DIRECTION ( 'NONE',  ( 1.000000000000000000, -0.000000000000000000, -0.000000000000000000 ) ) ;
#1083 = VERTEX_POINT ( 'NONE', #7685 ) ;
#1084 = CARTESIAN_POINT ( 'NONE',  ( -1.500000000000001332, 0.000000000000000000, 0.000000000000000000 ) ) ;
#1085 = PLANE ( 'NONE',  #3231 ) ;
#1086 = ORIENTED_EDGE ( 'NONE', *, *, #463, .T. ) ;
#1087 = DIRECTION ( 'NONE',  ( 0.000000000000000000, 0.000000000000000000, 1.000000000000000000 ) ) ;
#1088 = ORIENTED_EDGE ( 'NONE', *, *, #8797, .T. ) ;
#1089 = AXIS2_PLACEMENT_3D ( 'NONE', #3095, #10765, #8031 ) ;
#1090 = CYLINDRICAL_SURFACE ( 'NONE', #4198, 5.000000000000000000 ) ;
#1091 = DIRECTION ( 'NONE',  ( -1.000000000000000000, -0.000000000000000000, -0.000000000000000000 ) ) ;
#1092 = DIRECTION ( 'NONE',  ( 0.000000000000000000, 0.000000000000000000, -1.000000000000000000 ) ) ;
#1093 = CARTESIAN_POINT ( 'NONE',  ( 15.00000000000000355, 44.00000000000001421, 2.149999999999999023 ) ) ;
#1094 = VERTEX_POINT ( 'NONE', #10483 ) ;
#1095 = ORIENTED_EDGE ( 'NONE', *, *, #11677, .F. ) ;
#1096 = CIRCLE ( 'NONE', #10089, 12.49999999999999645 ) ;
#1097 =( NAMED_UNIT ( * ) PLANE_ANGLE_UNIT ( ) SI_UNIT ( $, .RADIAN. ) );
#1098 = ORIENTED_EDGE ( 'NONE', *, *, #10630, .F. ) ;
#1099 = DIRECTION ( 'NONE',  ( 0.000000000000000000, 0.000000000000000000, -1.000000000000000000 ) ) ;
#1100 = EDGE_CURVE ( 'NONE', #10975, #9875, #12343, .T. ) ;
#1101 = VERTEX_POINT ( 'NONE', #1046 ) ;
#1102 = EDGE_CURVE ( 'NONE', #10119, #2301, #6017, .T. ) ;
#1103 = ORIENTED_EDGE ( 'NONE', *, *, #8592, .T. ) ;
#1104 = EDGE_LOOP ( 'NONE', ( #1748, #5954 ) ) ;
#1105 = CARTESIAN_POINT ( 'NONE',  ( 4.999999999999999112, -9.168210874537443544, -18.05452603534175537 ) ) ;
#1106 = LINE ( 'NONE', #4917, #10396 ) ;
#1107 = DIRECTION ( 'NONE',  ( 1.000000000000000000, 0.000000000000000000, 0.000000000000000000 ) ) ;
#1108 = CARTESIAN_POINT ( 'NONE',  ( -10.00000000000000000, 0.000000000000000000, 0.000000000000000000 ) ) ;
#1109 = VERTEX_POINT ( 'NONE', #3735 ) ;
#1110 = DIRECTION ( 'NONE',  ( 1.000000000000000000, 0.000000000000000000, 0.000000000000000000 ) ) ;
#1111 = ORIENTED_EDGE ( 'NONE', *, *, #4167, .F. ) ;
#1112 = EDGE_CURVE ( 'NONE', #1842, #1155, #6743, .T. ) ;
#1113 =( NAMED_UNIT ( * ) PLANE_ANGLE_UNIT ( ) SI_UNIT ( $, .RADIAN. ) );
#1114 = ORIENTED_EDGE ( 'NONE', *, *, #7913, .T. ) ;
#1115 = DIRECTION ( 'NONE',  ( -1.000000000000000000, 0.000000000000000000, 0.000000000000000000 ) ) ;
#1116 = EDGE_CURVE ( 'NONE', #5049, #6113, #10419, .T. ) ;
#1117 = EDGE_LOOP ( 'NONE', ( #5523, #7085, #2430, #10564 ) ) ;
#1118 = FACE_OUTER_BOUND ( 'NONE', #12277, .T. ) ;
#1119 = EDGE_CURVE ( 'NONE', #1183, #3700, #1106, .T. ) ;
#1120 = DIRECTION ( 'NONE',  ( 0.000000000000000000, 0.9238795325112877377, -0.3826834323650873393 ) ) ;
#1121 = ORIENTED_EDGE ( 'NONE', *, *, #4874, .F. ) ;
#1122 = DIRECTION ( 'NONE',  ( 0.000000000000000000, 0.000000000000000000, 1.000000000000000000 ) ) ;
#1123 = DIRECTION ( 'NONE',  ( 0.000000000000000000, 0.000000000000000000, -1.000000000000000000 ) ) ;
#1124 = EDGE_LOOP ( 'NONE', ( #11736, #5228, #9752, #573 ) ) ;
#1125 = PRESENTATION_STYLE_ASSIGNMENT (( #9705 ) ) ;
#1126 = CARTESIAN_POINT ( 'NONE',  ( 26.00000000000000355, 0.000000000000000000, -41.99999999999999289 ) ) ;
#1127 = LINE ( 'NONE', #4997, #6703 ) ;
#1128 = ORIENTED_EDGE ( 'NONE', *, *, #8084, .T. ) ;
#1129 = DIRECTION ( 'NONE',  ( 0.000000000000000000, 0.4999999999999993894, -0.8660254037844389297 ) ) ;
#1130 = EDGE_CURVE ( 'NONE', #4691, #8601, #5008, .T. ) ;
#1131 = PRODUCT_DEFINITION_SHAPE ( 'NONE', 'NONE',  #7402 ) ;
#1132 = DIRECTION ( 'NONE',  ( 0.000000000000000000, 0.000000000000000000, 1.000000000000000000 ) ) ;
#1133 = LINE ( 'NONE', #3946, #10395 ) ;
#1134 = DIRECTION ( 'NONE',  ( 0.000000000000000000, 1.000000000000000000, -1.471414886128461471E-15 ) ) ;
#1135 = CARTESIAN_POINT ( 'NONE',  ( 25.00000000000000000, 0.000000000000000000, 0.000000000000000000 ) ) ;
#1136 = ORIENTED_EDGE ( 'NONE', *, *, #11866, .F. ) ;
#1137 = DIRECTION ( 'NONE',  ( 0.000000000000000000, 0.000000000000000000, -1.000000000000000000 ) ) ;
#1138 = ADVANCED_FACE ( 'NONE', ( #6614 ), #3794, .F. ) ;
#1139 = CARTESIAN_POINT ( 'NONE',  ( 0.000000000000000000, 0.000000000000000000, 0.000000000000000000 ) ) ;
#1140 = ADVANCED_FACE ( 'NONE', ( #160 ), #7801, .T. ) ;
#1141 = ORIENTED_EDGE ( 'NONE', *, *, #192, .F. ) ;
#1142 = FACE_OUTER_BOUND ( 'NONE', #11815, .T. ) ;
#1143 =( REPRESENTATION_RELATIONSHIP ('NONE','NONE', #9709, #678 ) REPRESENTATION_RELATIONSHIP_WITH_TRANSFORMATION ( #5786 )SHAPE_REPRESENTATION_RELATIONSHIP( ) );
#1144 = ORIENTED_EDGE ( 'NONE', *, *, #6176, .T. ) ;
#1145 = CARTESIAN_POINT ( 'NONE',  ( 1.500000000000001332, 0.000000000000000000, 0.000000000000000000 ) ) ;
#1146 = DIRECTION ( 'NONE',  ( 1.000000000000000000, 0.000000000000000000, 0.000000000000000000 ) ) ;
#1147 = LINE ( 'NONE', #6144, #1169 ) ;
#1148 = DIRECTION ( 'NONE',  ( -1.000000000000000000, -0.000000000000000000, -0.000000000000000000 ) ) ;
#1149 = DIRECTION ( 'NONE',  ( 0.000000000000000000, 0.000000000000000000, 1.000000000000000000 ) ) ;
#1150 = EDGE_LOOP ( 'NONE', ( #1280, #8719, #3599, #5364 ) ) ;
#1151 = ORIENTED_EDGE ( 'NONE', *, *, #2334, .F. ) ;
#1152 = DIRECTION ( 'NONE',  ( 0.000000000000000000, 1.000000000000000000, 0.000000000000000000 ) ) ;
#1153 = ORIENTED_EDGE ( 'NONE', *, *, #11492, .F. ) ;
#1154 = DIRECTION ( 'NONE',  ( 0.000000000000000000, 0.000000000000000000, 1.000000000000000000 ) ) ;
#1155 = VERTEX_POINT ( 'NONE', #7617 ) ;
#1156 = CARTESIAN_POINT ( 'NONE',  ( -26.00000000000000355, 0.000000000000000000, 0.000000000000000000 ) ) ;
#1157 = FACE_OUTER_BOUND ( 'NONE', #8222, .T. ) ;
#1158 = DIRECTION ( 'NONE',  ( 0.000000000000000000, 0.000000000000000000, -1.000000000000000000 ) ) ;
#1159 = LINE ( 'NONE', #11420, #417 ) ;
#1160 = ORIENTED_EDGE ( 'NONE', *, *, #3799, .T. ) ;
#1161 = VERTEX_POINT ( 'NONE', #7111 ) ;
#1162 = PRESENTATION_STYLE_ASSIGNMENT (( #3984 ) ) ;
#1163 = VERTEX_POINT ( 'NONE', #3116 ) ;
#1165 = CARTESIAN_POINT ( 'NONE',  ( 0.000000000000000000, 0.000000000000000000, 0.000000000000000000 ) ) ;
#1164 = AXIS2_PLACEMENT_3D ( 'NONE', #1603, #3421, #7254 ) ;
#1166 = CIRCLE ( 'NONE', #8970, 12.49999999999999645 ) ;
#1167 = ORIENTED_EDGE ( 'NONE', *, *, #4711, .F. ) ;
#1168 = DIRECTION ( 'NONE',  ( -1.000000000000000000, 0.000000000000000000, -0.000000000000000000 ) ) ;
#1169 = VECTOR ( 'NONE', #4027, 1000.000000000000000 ) ;
#1170 = DIRECTION ( 'NONE',  ( -0.000000000000000000, 0.000000000000000000, 1.000000000000000000 ) ) ;
#1171 = EDGE_CURVE ( 'NONE', #6684, #6331, #3612, .T. ) ;
#1172 = CIRCLE ( 'NONE', #4361, 5.000000000000000000 ) ;
#1173 = AXIS2_PLACEMENT_3D ( 'NONE', #5680, #1799, #5878 ) ;
#1174 = EDGE_CURVE ( 'NONE', #7662, #5539, #10599, .T. ) ;
#1175 = ORIENTED_EDGE ( 'NONE', *, *, #11942, .T. ) ;
#1176 = DIRECTION ( 'NONE',  ( 1.000000000000000000, 0.000000000000000000, 0.000000000000000000 ) ) ;
#1177 = PLANE ( 'NONE',  #1265 ) ;
#1178 = ORIENTED_EDGE ( 'NONE', *, *, #5787, .T. ) ;
#1179 = DIRECTION ( 'NONE',  ( 0.000000000000000000, 0.000000000000000000, 1.000000000000000000 ) ) ;
#1180 = SURFACE_STYLE_USAGE ( .BOTH. , #10695 ) ;
#1181 = FACE_OUTER_BOUND ( 'NONE', #4103, .T. ) ;
#1182 = CARTESIAN_POINT ( 'NONE',  ( 0.000000000000000000, 0.000000000000000000, 0.000000000000000000 ) ) ;
#1183 = VERTEX_POINT ( 'NONE', #2155 ) ;
#1184 = FACE_OUTER_BOUND ( 'NONE', #8896, .T. ) ;
#1185 = AXIS2_PLACEMENT_3D ( 'NONE', #8772, #199, #4012 ) ;
#1186 = AXIS2_PLACEMENT_3D ( 'NONE', #11628, #9942, #3140 ) ;
#1187 = AXIS2_PLACEMENT_3D ( 'NONE', #11842, #11660, #469 ) ;
#1188 = FILL_AREA_STYLE_COLOUR ( '', #3026 ) ;
#1189 = CARTESIAN_POINT ( 'NONE',  ( 2.499999999999999556, -22.05152472667118957, -15.57980286237495804 ) ) ;
#1190 = EDGE_CURVE ( 'NONE', #720, #7137, #8012, .T. ) ;
#1191 = ADVANCED_FACE ( 'NONE', ( #5103 ), #5223, .F. ) ;
#1192 = DIRECTION ( 'NONE',  ( 0.000000000000000000, 0.000000000000000000, 1.000000000000000000 ) ) ;
#1193 = DIRECTION ( 'NONE',  ( 0.000000000000000000, -0.9238795325112906243, 0.3826834323650805114 ) ) ;
#1194 = ADVANCED_FACE ( 'NONE', ( #5046 ), #8925, .T. ) ;
#1195 = AXIS2_PLACEMENT_3D ( 'NONE', #8343, #2710, #12206 ) ;
#1196 = EDGE_LOOP ( 'NONE', ( #10186, #2981, #11180, #8301 ) ) ;
#1197 = CARTESIAN_POINT ( 'NONE',  ( -15.00000000000000000, 40.00000000000000711, -2.149999999999999023 ) ) ;
#1198 = DIRECTION ( 'NONE',  ( -0.000000000000000000, 1.000000000000000000, -0.000000000000000000 ) ) ;
#1199 = VECTOR ( 'NONE', #1553, 1000.000000000000000 ) ;
#1200 = ORIENTED_EDGE ( 'NONE', *, *, #8303, .F. ) ;
#1201 = DIRECTION ( 'NONE',  ( -0.000000000000000000, -0.000000000000000000, -1.000000000000000000 ) ) ;
#1202 = ORIENTED_EDGE ( 'NONE', *, *, #2946, .F. ) ;
#1203 = CARTESIAN_POINT ( 'NONE',  ( 0.000000000000000000, 0.000000000000000000, 0.000000000000000000 ) ) ;
#1204 = VECTOR ( 'NONE', #3845, 1000.000000000000000 ) ;
#1205 = EDGE_CURVE ( 'NONE', #8601, #11755, #1409, .T. ) ;
#1206 = AXIS2_PLACEMENT_3D ( 'NONE', #6911, #2202, #10892 ) ;
#1207 = CIRCLE ( 'NONE', #8399, 7.200000000007202416 ) ;
#1208 = FILL_AREA_STYLE_COLOUR ( '', #7601 ) ;
#1209 = DIRECTION ( 'NONE',  ( 1.000000000000000000, 0.000000000000000000, 0.000000000000000000 ) ) ;
#1210 = CARTESIAN_POINT ( 'NONE',  ( 4.999999999999999112, 14.88411597386729213, 8.035066368449255592 ) ) ;
#1211 = CARTESIAN_POINT ( 'NONE',  ( 45.00000000000000000, 6.123233995736765296E-16, -5.000000000000000000 ) ) ;
#1212 = ORIENTED_EDGE ( 'NONE', *, *, #3860, .F. ) ;
#1213 = FILL_AREA_STYLE ('',( #6917 ) ) ;
#1214 = ORIENTED_EDGE ( 'NONE', *, *, #7345, .F. ) ;
#1215 = CARTESIAN_POINT ( 'NONE',  ( 26.00000000000000355, 7.960204194457796463E-16, -6.500000000000000888 ) ) ;
#1216 = APPLICATION_PROTOCOL_DEFINITION ( 'draft international standard', 'automotive_design', 1998, #10489 ) ;
#1217 = VERTEX_POINT ( 'NONE', #7980 ) ;
#1218 = VECTOR ( 'NONE', #8496, 1000.000000000000000 ) ;
#1219 = EDGE_CURVE ( 'NONE', #649, #7970, #3167, .T. ) ;
#1220 = ORIENTED_EDGE ( 'NONE', *, *, #12267, .F. ) ;
#1221 = VECTOR ( 'NONE', #9353, 1000.000000000000000 ) ;
#1222 = AXIS2_PLACEMENT_3D ( 'NONE', #2107, #1985, #1049 ) ;
#1223 = ORIENTED_EDGE ( 'NONE', *, *, #871, .T. ) ;
#1224 = AXIS2_PLACEMENT_3D ( 'NONE', #1581, #3763, #11268 ) ;
#1225 = CARTESIAN_POINT ( 'NONE',  ( 2.500000000000000000, -1.178949249685218303, -2.041999999999998039 ) ) ;
#1226 = CARTESIAN_POINT ( 'NONE',  ( 1.000000000000000000, 0.5999999999999998668, -3.826895796574397046 ) ) ;
#1227 = AXIS2_PLACEMENT_3D ( 'NONE', #4048, #5927, #7621 ) ;
#1228 = AXIS2_PLACEMENT_3D ( 'NONE', #480, #7310, #3543 ) ;
#1229 = CARTESIAN_POINT ( 'NONE',  ( 0.000000000000000000, 0.000000000000000000, 0.000000000000000000 ) ) ;
#1230 = DIRECTION ( 'NONE',  ( -1.000000000000000000, 0.000000000000000000, 0.000000000000000000 ) ) ;
#1231 = ORIENTED_EDGE ( 'NONE', *, *, #10376, .T. ) ;
#1232 = ORIENTED_EDGE ( 'NONE', *, *, #5271, .T. ) ;
#1233 =( NAMED_UNIT ( * ) PLANE_ANGLE_UNIT ( ) SI_UNIT ( $, .RADIAN. ) );
#1234 = VERTEX_POINT ( 'NONE', #9922 ) ;
#1235 = AXIS2_PLACEMENT_3D ( 'NONE', #1969, #9596, #149 ) ;
#1236 = DIRECTION ( 'NONE',  ( 0.000000000000000000, 0.000000000000000000, 1.000000000000000000 ) ) ;
#1237 = CIRCLE ( 'NONE', #4231, 2.396904916527700102 ) ;
#1238 = CIRCLE ( 'NONE', #8627, 2.690429798716874377 ) ;
#1239 = CARTESIAN_POINT ( 'NONE',  ( -25.39999999999996305, 0.000000000000000000, 2.000000000000000000 ) ) ;
#1240 = DIRECTION ( 'NONE',  ( -1.000000000000000000, 0.000000000000000000, 0.000000000000000000 ) ) ;
#1241 = AXIS2_PLACEMENT_3D ( 'NONE', #12123, #2513, #753 ) ;
#1242 = CIRCLE ( 'NONE', #7251, 7.200000000007201528 ) ;
#1243 = ORIENTED_EDGE ( 'NONE', *, *, #6959, .F. ) ;
#1244 = AXIS2_PLACEMENT_3D ( 'NONE', #11020, #571, #5466 ) ;
#1245 = CARTESIAN_POINT ( 'NONE',  ( 0.000000000000000000, 0.000000000000000000, 0.000000000000000000 ) ) ;
#1246 = DIRECTION ( 'NONE',  ( 0.000000000000000000, -1.000000000000000000, -1.048062100068272767E-14 ) ) ;
#1247 = ORIENTED_EDGE ( 'NONE', *, *, #1673, .T. ) ;
#1248 = LINE ( 'NONE', #5066, #837 ) ;
#1249 = LINE ( 'NONE', #5067, #4493 ) ;
#1250 = ADVANCED_FACE ( 'NONE', ( #10906 ), #12179, .T. ) ;
#1251 = ORIENTED_EDGE ( 'NONE', *, *, #4168, .T. ) ;
#1252 = CYLINDRICAL_SURFACE ( 'NONE', #5385, 9.600000000009600853 ) ;
#1253 = PRODUCT_DEFINITION_FORMATION_WITH_SPECIFIED_SOURCE ( 'ANY', '', #5415, .NOT_KNOWN. ) ;
#1254 = AXIS2_PLACEMENT_3D ( 'NONE', #5188, #4076, #9021 ) ;
#1255 = CIRCLE ( 'NONE', #7259, 27.00000000002699707 ) ;
#1256 = EDGE_CURVE ( 'NONE', #8750, #9748, #3233, .T. ) ;
#1257 = CIRCLE ( 'NONE', #10644, 20.24900000002024925 ) ;
#1258 = DIRECTION ( 'NONE',  ( -1.000000000000000000, 0.000000000000000000, 0.000000000000000000 ) ) ;
#1259 = LINE ( 'NONE', #5126, #11190 ) ;
#1260 = CARTESIAN_POINT ( 'NONE',  ( 4.999999999999999112, -15.22291137398912397, -14.46592441914980576 ) ) ;
#1261 = CARTESIAN_POINT ( 'NONE',  ( 37.00000000000000711, 1.456773409934505593E-31, -41.99999999999998579 ) ) ;
#1262 = DIRECTION ( 'NONE',  ( -1.000000000000000000, 0.000000000000000000, 0.000000000000000000 ) ) ;
#1263 = VERTEX_POINT ( 'NONE', #4281 ) ;
#1264 = DIRECTION ( 'NONE',  ( 1.000000000000000000, -0.000000000000000000, 0.000000000000000000 ) ) ;
#1265 = AXIS2_PLACEMENT_3D ( 'NONE', #4992, #8819, #247 ) ;
#1266 = CARTESIAN_POINT ( 'NONE',  ( 0.000000000000000000, 0.000000000000000000, 5.000000000000000000 ) ) ;
#1267 = ORIENTED_EDGE ( 'NONE', *, *, #10956, .F. ) ;
#1268 = DIRECTION ( 'NONE',  ( 0.000000000000000000, 0.000000000000000000, 1.000000000000000000 ) ) ;
#1269 = EDGE_CURVE ( 'NONE', #6377, #11243, #6158, .T. ) ;
#1270 = VERTEX_POINT ( 'NONE', #4974 ) ;
#1271 = CARTESIAN_POINT ( 'NONE',  ( -36.00000000000000711, 0.000000000000000000, 0.000000000000000000 ) ) ;
#1272 = EDGE_CURVE ( 'NONE', #4406, #9587, #10993, .T. ) ;
#1273 = EDGE_CURVE ( 'NONE', #6083, #7961, #3680, .T. ) ;
#1274 = CIRCLE ( 'NONE', #4467, 7.200000000007204193 ) ;
#1275 = PRESENTATION_STYLE_ASSIGNMENT (( #3337 ) ) ;
#1276 = DIRECTION ( 'NONE',  ( -0.000000000000000000, 1.000000000000000000, -0.000000000000000000 ) ) ;
#1277 = CARTESIAN_POINT ( 'NONE',  ( 0.000000000000000000, 4.769696007084728073, 1.500000000000000000 ) ) ;
#1278 = CARTESIAN_POINT ( 'NONE',  ( 4.999999999999999112, 17.79862902732283914, -13.85025647830039119 ) ) ;
#1279 = ORIENTED_EDGE ( 'NONE', *, *, #11894, .T. ) ;
#1280 = ORIENTED_EDGE ( 'NONE', *, *, #939, .F. ) ;
#1281 = CARTESIAN_POINT ( 'NONE',  ( -15.00000000000000000, 44.00000000000001421, 2.149999999999999023 ) ) ;
#1282 = CIRCLE ( 'NONE', #5483, 27.00000000002699707 ) ;
#1283 = ORIENTED_EDGE ( 'NONE', *, *, #11655, .F. ) ;
#1284 = PRODUCT_RELATED_PRODUCT_CATEGORY ( 'part', '', ( #10302 ) ) ;
#1285 = CARTESIAN_POINT ( 'NONE',  ( 0.000000000000000000, 0.000000000000000000, 6.250000000000000000 ) ) ;
#1286 = FACE_OUTER_BOUND ( 'NONE', #2294, .T. ) ;
#1287 = DIRECTION ( 'NONE',  ( 0.000000000000000000, 0.8620420264545162192, 0.5068368027542899945 ) ) ;
#1288 = CIRCLE ( 'NONE', #1089, 40.00000000000000711 ) ;
#1289 = CARTESIAN_POINT ( 'NONE',  ( -10.00000000000000000, 0.000000000000000000, 0.000000000000000000 ) ) ;
#1290 = CARTESIAN_POINT ( 'NONE',  ( 4.999999999999999112, 0.000000000000000000, 0.000000000000000000 ) ) ;
#1291 = ORIENTED_EDGE ( 'NONE', *, *, #1273, .T. ) ;
#1292 = ORIENTED_EDGE ( 'NONE', *, *, #11905, .T. ) ;
#1293 =( LENGTH_UNIT ( ) NAMED_UNIT ( * ) SI_UNIT ( .MILLI., .METRE. ) );
#1294 = EDGE_CURVE ( 'NONE', #5455, #1899, #2602, .T. ) ;
#1296 = ADVANCED_FACE ( 'NONE', ( #8876 ), #8059, .T. ) ;
#1295 = ORIENTED_EDGE ( 'NONE', *, *, #9386, .F. ) ;
#1297 = CARTESIAN_POINT ( 'NONE',  ( 4.999999999999999112, 0.000000000000000000, 0.000000000000000000 ) ) ;
#1298 = AXIS2_PLACEMENT_3D ( 'NONE', #8826, #184, #9826 ) ;
#1299 = CARTESIAN_POINT ( 'NONE',  ( 33.00000000000000000, 9.184850993605149917E-16, 7.500000000000000888 ) ) ;
#1300 = LINE ( 'NONE', #3182, #1608 ) ;
#1301 = ORIENTED_EDGE ( 'NONE', *, *, #2405, .T. ) ;
#1302 = AXIS2_PLACEMENT_3D ( 'NONE', #7190, #9080, #11912 ) ;
#1303 = CARTESIAN_POINT ( 'NONE',  ( 0.000000000000000000, 0.000000000000000000, 0.000000000000000000 ) ) ;
#1304 = CARTESIAN_POINT ( 'NONE',  ( -36.00000000000000000, 40.00000000000000711, 20.00000000000001066 ) ) ;
#1305 = VERTEX_POINT ( 'NONE', #11844 ) ;
#1306 = DIRECTION ( 'NONE',  ( 0.000000000000000000, 0.000000000000000000, 1.000000000000000000 ) ) ;
#1307 = DIRECTION ( 'NONE',  ( 1.000000000000000000, -4.770489558936236458E-18, 6.855277276495153692E-34 ) ) ;
#1308 = ORIENTED_EDGE ( 'NONE', *, *, #4840, .T. ) ;
#1309 = CARTESIAN_POINT ( 'NONE',  ( 51.00000000000000000, 0.000000000000000000, -41.99999999999999289 ) ) ;
#1310 = DIRECTION ( 'NONE',  ( 0.000000000000000000, 0.000000000000000000, -1.000000000000000000 ) ) ;
#1311 = DIRECTION ( 'NONE',  ( 1.000000000000000000, 0.000000000000000000, 0.000000000000000000 ) ) ;
#1312 = DIRECTION ( 'NONE',  ( 0.000000000000000000, -1.000000000000000000, 1.287488025362403787E-15 ) ) ;
#1313 = DIRECTION ( 'NONE',  ( 0.000000000000000000, 0.000000000000000000, 1.000000000000000000 ) ) ;
#1314 = FACE_OUTER_BOUND ( 'NONE', #4071, .T. ) ;
#1315 = EDGE_LOOP ( 'NONE', ( #8246, #5545, #4189, #9435 ) ) ;
#1316 = ORIENTED_EDGE ( 'NONE', *, *, #2888, .F. ) ;
#1317 = EDGE_CURVE ( 'NONE', #2662, #10589, #3298, .T. ) ;
#1318 = LINE ( 'NONE', #7616, #9969 ) ;
#1319 = CYLINDRICAL_SURFACE ( 'NONE', #1431, 7.200000000007202416 ) ;
#1320 = VERTEX_POINT ( 'NONE', #4590 ) ;
#1321 = PLANE ( 'NONE',  #8288 ) ;
#1322 = ORIENTED_EDGE ( 'NONE', *, *, #9322, .T. ) ;
#1323 = FACE_OUTER_BOUND ( 'NONE', #4345, .T. ) ;
#1324 = CARTESIAN_POINT ( 'NONE',  ( 4.999999999999999112, -8.527191590521155717, 11.41582255376070343 ) ) ;
#1325 = CARTESIAN_POINT ( 'NONE',  ( -36.00000000000000711, 0.000000000000000000, 6.500000000000000888 ) ) ;
#1326 = EDGE_CURVE ( 'NONE', #4084, #5310, #9616, .T. ) ;
#1327 = DIRECTION ( 'NONE',  ( 0.000000000000000000, 0.000000000000000000, -1.000000000000000000 ) ) ;
#1328 = CARTESIAN_POINT ( 'NONE',  ( 26.00000000000000355, 12.50000000000000000, -24.50000000000000000 ) ) ;
#1329 = ORIENTED_EDGE ( 'NONE', *, *, #10497, .T. ) ;
#1330 = ADVANCED_FACE ( 'NONE', ( #11038, #1531 ), #4403, .T. ) ;
#1331 = CARTESIAN_POINT ( 'NONE',  ( -26.00000000000000355, 34.64101615137756340, -19.99999999999998934 ) ) ;
#1332 = EDGE_CURVE ( 'NONE', #9795, #6083, #1421, .T. ) ;
#1333 = VERTEX_POINT ( 'NONE', #2658 ) ;
#1334 = CARTESIAN_POINT ( 'NONE',  ( 4.999999999999999112, 0.000000000000000000, 20.24900000002024569 ) ) ;
#1335 = ITEM_DEFINED_TRANSFORMATION ( 'NONE', 'NONE', #9445,  #6056 ) ;
#1336 = ORIENTED_EDGE ( 'NONE', *, *, #10129, .T. ) ;
#1337 = CARTESIAN_POINT ( 'NONE',  ( -3.309651814758565180, -5.455921364805393026, -1.000000000000000000 ) ) ;
#1338 = DIRECTION ( 'NONE',  ( 1.000000000000000000, 0.000000000000000000, 0.000000000000000000 ) ) ;
#1339 = CARTESIAN_POINT ( 'NONE',  ( 0.000000000000000000, 16.90755573046746107, -0.4834863907626340551 ) ) ;
#1340 = CARTESIAN_POINT ( 'NONE',  ( 4.999999999999999112, -8.527191590521155717, 11.41582255376070343 ) ) ;
#1341 = CARTESIAN_POINT ( 'NONE',  ( -15.00000000000000000, 40.00000000000000711, -2.000000000000000000 ) ) ;
#1342 = ORIENTED_EDGE ( 'NONE', *, *, #12054, .T. ) ;
#1343 = ADVANCED_FACE ( 'NONE', ( #5477 ), #10276, .T. ) ;
#1344 = ADVANCED_FACE ( 'NONE', ( #3533 ), #12207, .T. ) ;
#1345 = CARTESIAN_POINT ( 'NONE',  ( 0.000000000000000000, 0.5999999999999998668, 4.000000000000000000 ) ) ;
#1346 = ADVANCED_FACE ( 'NONE', ( #7351 ), #7413, .T. ) ;
#1347 = VERTEX_POINT ( 'NONE', #9237 ) ;
#1348 = DIRECTION ( 'NONE',  ( 1.000000000000000000, 0.000000000000000000, 0.000000000000000000 ) ) ;
#1349 = ORIENTED_EDGE ( 'NONE', *, *, #3855, .T. ) ;
#1350 = DIRECTION ( 'NONE',  ( 1.000000000000000000, -0.000000000000000000, -0.000000000000000000 ) ) ;
#1351 = FACE_OUTER_BOUND ( 'NONE', #198, .T. ) ;
#1352 = CARTESIAN_POINT ( 'NONE',  ( 50.00005079999999680, 0.000000000000000000, 0.000000000000000000 ) ) ;
#1353 = ADVANCED_FACE ( 'NONE', ( #8293 ), #12082, .T. ) ;
#1354 = EDGE_CURVE ( 'NONE', #6904, #11926, #7299, .T. ) ;
#1355 = EDGE_LOOP ( 'NONE', ( #8062, #7066, #782, #5091 ) ) ;
#1356 = CARTESIAN_POINT ( 'NONE',  ( 1.000000000000000000, 0.000000000000000000, 0.000000000000000000 ) ) ;
#1357 = VECTOR ( 'NONE', #5618, 1000.000000000000000 ) ;
#1358 = VERTEX_POINT ( 'NONE', #5530 ) ;
#1359 = CYLINDRICAL_SURFACE ( 'NONE', #8438, 9.600000000009600853 ) ;
#1360 = AXIS2_PLACEMENT_3D ( 'NONE', #1518, #7397, #1701 ) ;
#1361 = FACE_OUTER_BOUND ( 'NONE', #8791, .T. ) ;
#1362 = EDGE_LOOP ( 'NONE', ( #3805, #3426, #3636, #11704 ) ) ;
#1363 = LINE ( 'NONE', #433, #6985 ) ;
#1364 = VECTOR ( 'NONE', #12094, 1000.000000000000000 ) ;
#1365 = VECTOR ( 'NONE', #10802, 1000.000000000000000 ) ;
#1366 = SURFACE_STYLE_USAGE ( .BOTH. , #6190 ) ;
#1367 = EDGE_CURVE ( 'NONE', #644, #4373, #5215, .T. ) ;
#1368 = CYLINDRICAL_SURFACE ( 'NONE', #11978, 7.000000000000004441 ) ;
#1369 = DIRECTION ( 'NONE',  ( 1.000000000000000000, -0.000000000000000000, -0.000000000000000000 ) ) ;
#1370 = CARTESIAN_POINT ( 'NONE',  ( 36.00000000000000711, 4.210917358895616580, 2.303947698310782943 ) ) ;
#1371 = CARTESIAN_POINT ( 'NONE',  ( 4.999999999999999112, -20.41639017900862996, 4.916402349214511247 ) ) ;
#1372 = ORIENTED_EDGE ( 'NONE', *, *, #965, .T. ) ;
#1373 = EDGE_LOOP ( 'NONE', ( #11318, #8359, #9664, #4705 ) ) ;
#1374 = FACE_BOUND ( 'NONE', #7631, .T. ) ;
#1375 = PLANE ( 'NONE',  #5221 ) ;
#1376 = AXIS2_PLACEMENT_3D ( 'NONE', #318, #6136, #11817 ) ;
#1377 = ORIENTED_EDGE ( 'NONE', *, *, #7727, .F. ) ;
#1378 = DIRECTION ( 'NONE',  ( 0.000000000000000000, 0.8772744497699203059, 0.4799891038147465760 ) ) ;
#1379 = PRODUCT_DEFINITION_CONTEXT ( 'detailed design', #11353, 'design' ) ;
#1380 = AXIS2_PLACEMENT_3D ( 'NONE', #5498, #2540, #4425 ) ;
#1381 = ORIENTED_EDGE ( 'NONE', *, *, #5937, .F. ) ;
#1382 = FACE_BOUND ( 'NONE', #11416, .T. ) ;
#1383 = CIRCLE ( 'NONE', #10367, 14.24900000001425582 ) ;
#1384 = CIRCLE ( 'NONE', #12155, 7.200000000007202416 ) ;
#1385 = DIRECTION ( 'NONE',  ( -1.000000000000000000, 0.000000000000000000, -0.000000000000000000 ) ) ;
#1386 = CARTESIAN_POINT ( 'NONE',  ( 4.999999999999999112, -1.676853263447986242, 14.14998813191269100 ) ) ;
#1387 = CIRCLE ( 'NONE', #2782, 20.24900000002024925 ) ;
#1388 = CIRCLE ( 'NONE', #2388, 20.24900000002024925 ) ;
#1389 = CARTESIAN_POINT ( 'NONE',  ( 0.000000000000000000, 0.000000000000000000, 0.000000000000000000 ) ) ;
#1390 = CARTESIAN_POINT ( 'NONE',  ( 1.000000000000000000, 0.5999999999999998668, 4.000000000000000000 ) ) ;
#1391 = EDGE_LOOP ( 'NONE', ( #5800, #10273, #5602, #1812 ) ) ;
#1392 = CARTESIAN_POINT ( 'NONE',  ( 2.500000000000000000, -1.178949249685213863, 2.042000000000002924 ) ) ;
#1393 = ORIENTED_EDGE ( 'NONE', *, *, #1585, .T. ) ;
#1394 = FACE_BOUND ( 'NONE', #860, .T. ) ;
#1395 = ORIENTED_EDGE ( 'NONE', *, *, #8716, .F. ) ;
#1396 = AXIS2_PLACEMENT_3D ( 'NONE', #10523, #4715, #4770 ) ;
#1397 = EDGE_CURVE ( 'NONE', #8903, #2114, #6531, .T. ) ;
#1398 = AXIS2_PLACEMENT_3D ( 'NONE', #7378, #9379, #9195 ) ;
#1399 = EDGE_CURVE ( 'NONE', #7808, #11273, #6221, .T. ) ;
#1400 = DIRECTION ( 'NONE',  ( 0.000000000000000000, 0.000000000000000000, -1.000000000000000000 ) ) ;
#1401 = LINE ( 'NONE', #5222, #8999 ) ;
#1402 = CARTESIAN_POINT ( 'NONE',  ( 25.00000000000000000, 0.000000000000000000, 0.000000000000000000 ) ) ;
#1403 = DIRECTION ( 'NONE',  ( 1.000000000000000000, 0.000000000000000000, 0.000000000000000000 ) ) ;
#1404 = FACE_OUTER_BOUND ( 'NONE', #11301, .T. ) ;
#1405 = AXIS2_PLACEMENT_3D ( 'NONE', #5087, #325, #9907 ) ;
#1406 = ORIENTED_EDGE ( 'NONE', *, *, #8447, .F. ) ;
#1407 = VECTOR ( 'NONE', #1312, 1000.000000000000000 ) ;
#1408 = DIRECTION ( 'NONE',  ( 0.000000000000000000, 0.000000000000000000, 1.000000000000000000 ) ) ;
#1409 = CIRCLE ( 'NONE', #1619, 7.200000000007201528 ) ;
#1410 = ORIENTED_EDGE ( 'NONE', *, *, #6663, .T. ) ;
#1411 = CARTESIAN_POINT ( 'NONE',  ( 0.000000000000000000, 0.000000000000000000, 0.000000000000000000 ) ) ;
#1412 = ORIENTED_EDGE ( 'NONE', *, *, #980, .F. ) ;
#1413 = DIRECTION ( 'NONE',  ( 0.000000000000000000, 0.000000000000000000, -1.000000000000000000 ) ) ;
#1414 = ADVANCED_FACE ( 'NONE', ( #3479 ), #2525, .T. ) ;
#1415 = CARTESIAN_POINT ( 'NONE',  ( 37.00000000000000711, 0.000000000000000000, 0.000000000000000000 ) ) ;
#1416 = AXIS2_PLACEMENT_3D ( 'NONE', #10510, #133, #4890 ) ;
#1417 = CIRCLE ( 'NONE', #11191, 40.00000000000000711 ) ;
#1418 = ADVANCED_FACE ( 'NONE', ( #9115 ), #8166, .F. ) ;
#1419 = AXIS2_PLACEMENT_3D ( 'NONE', #10858, #1230, #5105 ) ;
#1420 = EDGE_CURVE ( 'NONE', #3057, #6849, #10157, .T. ) ;
#1421 = CIRCLE ( 'NONE', #7422, 2.690429798716874377 ) ;
#1422 = AXIS2_PLACEMENT_3D ( 'NONE', #4926, #236, #11538 ) ;
#1423 = EDGE_CURVE ( 'NONE', #6198, #5296, #11216, .T. ) ;
#1424 = VERTEX_POINT ( 'NONE', #11327 ) ;
#1425 = CARTESIAN_POINT ( 'NONE',  ( 36.00000000000000711, 3.277848209564065307, -38.49347592122088457 ) ) ;
#1426 = ORIENTED_EDGE ( 'NONE', *, *, #4016, .T. ) ;
#1428 = CARTESIAN_POINT ( 'NONE',  ( 0.000000000000000000, -1.178949249685213863, 2.042000000000002924 ) ) ;
#1427 = COLOUR_RGB ( '',0.8941176470588234615, 0.8941176470588234615, 0.8941176470588234615 ) ;
#1429 = AXIS2_PLACEMENT_3D ( 'NONE', #4339, #8060, #11774 ) ;
#1430 = VERTEX_POINT ( 'NONE', #1968 ) ;
#1431 = AXIS2_PLACEMENT_3D ( 'NONE', #7204, #3149, #9844 ) ;
#1432 = SHAPE_REPRESENTATION_RELATIONSHIP ( 'NONE' , 'NONE' ,  #11292, #12103 ) ;
#1433 = CIRCLE ( 'NONE', #10025, 4.250000000000000000 ) ;
#1434 = CARTESIAN_POINT ( 'NONE',  ( -36.00000000000000711, 34.64101615137756340, -19.99999999999998934 ) ) ;
#1435 = CIRCLE ( 'NONE', #2619, 7.399999999999999467 ) ;
#1436 = FACE_OUTER_BOUND ( 'NONE', #11778, .T. ) ;
#1437 = ADVANCED_FACE ( 'NONE', ( #10586, #10331 ), #8536, .T. ) ;
#1438 = ORIENTED_EDGE ( 'NONE', *, *, #6782, .T. ) ;
#1439 = CARTESIAN_POINT ( 'NONE',  ( 2.500000000000000000, 0.000000000000000000, 0.000000000000000000 ) ) ;
#1440 = MECHANICAL_DESIGN_GEOMETRIC_PRESENTATION_REPRESENTATION (  '', ( #7846 ), #10219 ) ;
#1441 = VECTOR ( 'NONE', #9727, 1000.000000000000000 ) ;
#1442 = CIRCLE ( 'NONE', #4643, 2.041999999999999815 ) ;
#1443 = FACE_OUTER_BOUND ( 'NONE', #4634, .T. ) ;
#1444 = AXIS2_PLACEMENT_3D ( 'NONE', #316, #443, #11744 ) ;
#1445 = DIRECTION ( 'NONE',  ( 1.000000000000000000, 0.000000000000000000, 0.000000000000000000 ) ) ;
#1446 = CARTESIAN_POINT ( 'NONE',  ( 4.999999999999999112, 18.05452603534165945, 9.168210874537644273 ) ) ;
#1447 = LINE ( 'NONE', #442, #256 ) ;
#1448 = LINE ( 'NONE', #5263, #7664 ) ;
#1449 = VERTEX_POINT ( 'NONE', #2770 ) ;
#1450 = ORIENTED_EDGE ( 'NONE', *, *, #11721, .T. ) ;
#1451 = CARTESIAN_POINT ( 'NONE',  ( 0.1191357322639439581, -0.5999999999999995337, -3.174145254273323058 ) ) ;
#1452 =( NAMED_UNIT ( * ) PLANE_ANGLE_UNIT ( ) SI_UNIT ( $, .RADIAN. ) );
#1453 = LINE ( 'NONE', #6137, #3433 ) ;
#1454 = AXIS2_PLACEMENT_3D ( 'NONE', #2754, #3707, #2640 ) ;
#1455 = VERTEX_POINT ( 'NONE', #3909 ) ;
#1456 = DIRECTION ( 'NONE',  ( 0.000000000000000000, 0.000000000000000000, 1.000000000000000000 ) ) ;
#1457 = CIRCLE ( 'NONE', #654, 6.000000000000005329 ) ;
#1458 = ADVANCED_FACE ( 'NONE', ( #2845 ), #8721, .T. ) ;
#1459 = AXIS2_PLACEMENT_3D ( 'NONE', #3562, #10932, #9198 ) ;
#1460 = VERTEX_POINT ( 'NONE', #2030 ) ;
#1461 = LINE ( 'NONE', #2142, #10026 ) ;
#1462 = EDGE_CURVE ( 'NONE', #3276, #644, #4904, .T. ) ;
#1463 = ORIENTED_EDGE ( 'NONE', *, *, #1219, .T. ) ;
#1464 = VECTOR ( 'NONE', #5009, 1000.000000000000000 ) ;
#1465 = CARTESIAN_POINT ( 'NONE',  ( 36.00000000000000711, 6.123233995736765296E-16, -5.000000000000000000 ) ) ;
#1466 = AXIS2_PLACEMENT_3D ( 'NONE', #11729, #5998, #9819 ) ;
#1467 = DIRECTION ( 'NONE',  ( -1.000000000000000000, -0.000000000000000000, -0.000000000000000000 ) ) ;
#1468 = CARTESIAN_POINT ( 'NONE',  ( 36.00000000000000000, 30.00000000000000711, -19.99999999999998934 ) ) ;
#1469 = ORIENTED_EDGE ( 'NONE', *, *, #1219, .F. ) ;
#1470 = CARTESIAN_POINT ( 'NONE',  ( -20.00000000000000000, 0.000000000000000000, 0.000000000000000000 ) ) ;
#1471 = DIRECTION ( 'NONE',  ( 1.000000000000000000, 0.000000000000000000, 0.000000000000000000 ) ) ;
#1472 = ORIENTED_EDGE ( 'NONE', *, *, #11211, .F. ) ;
#1473 = DIRECTION ( 'NONE',  ( 0.000000000000000000, -1.000000000000000000, 0.000000000000000000 ) ) ;
#1474 = EDGE_LOOP ( 'NONE', ( #4560, #11323, #11816, #11431 ) ) ;
#1475 = VECTOR ( 'NONE', #803, 1000.000000000000000 ) ;
#1476 = CARTESIAN_POINT ( 'NONE',  ( 4.999999999999999112, -1.676853263447787068, -14.14998813191271410 ) ) ;
#1477 = LINE ( 'NONE', #6107, #6590 ) ;
#1478 = DIRECTION ( 'NONE',  ( -1.000000000000000000, 0.000000000000000000, 0.000000000000000000 ) ) ;
#1479 = DIRECTION ( 'NONE',  ( 0.000000000000000000, 0.000000000000000000, 1.000000000000000000 ) ) ;
#1480 = DIRECTION ( 'NONE',  ( 0.000000000000000000, -0.5446390350150287496, 0.8386705679454229401 ) ) ;
#1481 = ORIENTED_EDGE ( 'NONE', *, *, #6301, .T. ) ;
#1482 = AXIS2_PLACEMENT_3D ( 'NONE', #522, #7226, #11143 ) ;
#1483 = DIRECTION ( 'NONE',  ( -1.000000000000000000, -0.000000000000000000, -0.000000000000000000 ) ) ;
#1484 = ORIENTED_EDGE ( 'NONE', *, *, #6864, .F. ) ;
#1485 = ADVANCED_FACE ( 'NONE', ( #146 ), #1910, .F. ) ;
#1486 = DIRECTION ( 'NONE',  ( 2.775557561562891351E-17, -0.6749244146946962175, -0.7378868710371676576 ) ) ;
#1487 = ORIENTED_EDGE ( 'NONE', *, *, #1520, .T. ) ;
#1488 = CARTESIAN_POINT ( 'NONE',  ( 0.000000000000000000, 13.85025647830057416, 17.79862902732270413 ) ) ;
#1489 = LINE ( 'NONE', #9124, #6369 ) ;
#1490 = AXIS2_PLACEMENT_3D ( 'NONE', #5654, #5711, #9588 ) ;
#1491 = VERTEX_POINT ( 'NONE', #7725 ) ;
#1492 = FACE_OUTER_BOUND ( 'NONE', #2999, .T. ) ;
#1493 = EDGE_CURVE ( 'NONE', #4719, #7642, #3775, .T. ) ;
#1494 = VERTEX_POINT ( 'NONE', #6594 ) ;
#1495 = ORIENTED_EDGE ( 'NONE', *, *, #595, .F. ) ;
#1496 = EDGE_CURVE ( 'NONE', #8928, #3677, #566, .T. ) ;
#1497 = EDGE_CURVE ( 'NONE', #8881, #432, #11394, .T. ) ;
#1498 = DIRECTION ( 'NONE',  ( 0.000000000000000000, 0.000000000000000000, -1.000000000000000000 ) ) ;
#1499 = ORIENTED_EDGE ( 'NONE', *, *, #4582, .T. ) ;
#1500 = CARTESIAN_POINT ( 'NONE',  ( 4.999999999999999112, 9.168210874537576771, 18.05452603534168432 ) ) ;
#1501 = DIRECTION ( 'NONE',  ( 1.000000000000000000, 0.000000000000000000, 0.000000000000000000 ) ) ;
#1502 = AXIS2_PLACEMENT_3D ( 'NONE', #8370, #12162, #3617 ) ;
#1503 = DIRECTION ( 'NONE',  ( 1.301452268327822979E-17, 0.7707772616747329275, 0.6371047110838219396 ) ) ;
#1504 = CARTESIAN_POINT ( 'NONE',  ( 29.00000000000000000, 0.000000000000000000, -41.99999999999999289 ) ) ;
#1505 = DIRECTION ( 'NONE',  ( 1.000000000000000000, 0.000000000000000000, 0.000000000000000000 ) ) ;
#1506 = CARTESIAN_POINT ( 'NONE',  ( 4.999999999999999112, -14.40062958310459251, -8.872489362018340486 ) ) ;
#1507 = ORIENTED_EDGE ( 'NONE', *, *, #10328, .T. ) ;
#1508 = ORIENTED_EDGE ( 'NONE', *, *, #7159, .T. ) ;
#1509 = DIRECTION ( 'NONE',  ( -1.000000000000000000, 0.000000000000000000, -0.000000000000000000 ) ) ;
#1510 =( NAMED_UNIT ( * ) SI_UNIT ( $, .STERADIAN. ) SOLID_ANGLE_UNIT ( ) );
#1511 = CARTESIAN_POINT ( 'NONE',  ( 26.00000000000000355, 0.000000000000000000, 0.000000000000000000 ) ) ;
#1512 = PRODUCT_RELATED_PRODUCT_CATEGORY ( 'part', '', ( #6628 ) ) ;
#1513 = EDGE_LOOP ( 'NONE', ( #1666, #2104, #8806 ) ) ;
#1514 = DIRECTION ( 'NONE',  ( 0.000000000000000000, 0.000000000000000000, -1.000000000000000000 ) ) ;
#1515 = ORIENTED_EDGE ( 'NONE', *, *, #7216, .T. ) ;
#1516 = DIRECTION ( 'NONE',  ( 0.000000000000000000, 0.000000000000000000, 1.000000000000000000 ) ) ;
#1517 = ORIENTED_EDGE ( 'NONE', *, *, #6223, .T. ) ;
#1518 = CARTESIAN_POINT ( 'NONE',  ( 0.000000000000000000, 0.000000000000000000, 0.000000000000000000 ) ) ;
#1519 = EDGE_CURVE ( 'NONE', #31, #5277, #9169, .T. ) ;
#1520 = EDGE_CURVE ( 'NONE', #8668, #2987, #10467, .T. ) ;
#1521 = CARTESIAN_POINT ( 'NONE',  ( 36.00000000000000711, 0.000000000000000000, 40.00000000000000711 ) ) ;
#1522 = LINE ( 'NONE', #9285, #12208 ) ;
#1523 = ORIENTED_EDGE ( 'NONE', *, *, #712, .T. ) ;
#1524 = DIRECTION ( 'NONE',  ( 0.000000000000000000, 0.000000000000000000, 1.000000000000000000 ) ) ;
#1525 = DIRECTION ( 'NONE',  ( -0.000000000000000000, 0.8386705679454227180, 0.5446390350150290827 ) ) ;
#1526 = ORIENTED_EDGE ( 'NONE', *, *, #3195, .T. ) ;
#1527 = CARTESIAN_POINT ( 'NONE',  ( 2.500000000000000000, -2.357898499370432610, 3.252606517456513302E-15 ) ) ;
#1528 = VERTEX_POINT ( 'NONE', #5660 ) ;
#1529 = DIRECTION ( 'NONE',  ( -0.000000000000000000, -0.000000000000000000, -1.000000000000000000 ) ) ;
#1530 = CARTESIAN_POINT ( 'NONE',  ( 0.000000000000000000, 8.527191590521233877, -11.41582255376064126 ) ) ;
#1531 = FACE_OUTER_BOUND ( 'NONE', #8588, .T. ) ;
#1532 = DIRECTION ( 'NONE',  ( -1.000000000000000000, 0.000000000000000000, 0.000000000000000000 ) ) ;
#1533 = DIRECTION ( 'NONE',  ( -1.000000000000000000, 0.000000000000000000, 0.000000000000000000 ) ) ;
#1534 = ORIENTED_EDGE ( 'NONE', *, *, #4320, .F. ) ;
#1535 = DIRECTION ( 'NONE',  ( -0.000000000000000000, 1.000000000000000000, 0.000000000000000000 ) ) ;
#1536 = EDGE_CURVE ( 'NONE', #5049, #317, #11146, .T. ) ;
#1537 = ORIENTED_EDGE ( 'NONE', *, *, #1354, .F. ) ;
#1538 = CARTESIAN_POINT ( 'NONE',  ( 1.500000000000001332, 8.266365894244634333E-16, 6.750000000000000000 ) ) ;
#1539 = EDGE_LOOP ( 'NONE', ( #8919, #12318 ) ) ;
#1540 = DIRECTION ( 'NONE',  ( -1.000000000000000000, 0.000000000000000000, 0.000000000000000000 ) ) ;
#1541 = CARTESIAN_POINT ( 'NONE',  ( 4.999999999999999112, 0.000000000000000000, 0.000000000000000000 ) ) ;
#1542 = ORIENTED_EDGE ( 'NONE', *, *, #447, .F. ) ;
#1543 = CARTESIAN_POINT ( 'NONE',  ( 1.250000000000000000, -6.429618962271402616, 0.000000000000000000 ) ) ;
#1544 = SHAPE_REPRESENTATION ( 'plain washer 10669 type nl_iso_ISO 10669-5.4-N', ( #6056 ), #8843 ) ;
#1545 = ORIENTED_EDGE ( 'NONE', *, *, #3493, .F. ) ;
#1546 = CARTESIAN_POINT ( 'NONE',  ( 43.00000000000000000, 3.903127820947864496E-18, 0.000000000000000000 ) ) ;
#1547 = ORIENTED_EDGE ( 'NONE', *, *, #4092, .F. ) ;
#1548 =( LENGTH_UNIT ( ) NAMED_UNIT ( * ) SI_UNIT ( .MILLI., .METRE. ) );
#1549 = PLANE ( 'NONE',  #4101 ) ;
#1550 = ORIENTED_EDGE ( 'NONE', *, *, #10879, .T. ) ;
#1551 = CARTESIAN_POINT ( 'NONE',  ( 4.999999999999999112, 0.000000000000000000, 0.000000000000000000 ) ) ;
#1552 = ADVANCED_FACE ( 'NONE', ( #6730, #2960 ), #4771, .F. ) ;
#1553 = DIRECTION ( 'NONE',  ( 1.000000000000000000, -0.000000000000000000, -0.000000000000000000 ) ) ;
#1554 = EDGE_CURVE ( 'NONE', #1926, #8328, #9361, .T. ) ;
#1555 = CARTESIAN_POINT ( 'NONE',  ( 0.000000000000000000, 0.4834863907625768231, 16.90755573046746463 ) ) ;
#1556 = AXIS2_PLACEMENT_3D ( 'NONE', #9594, #1026, #6964 ) ;
#1557 = CARTESIAN_POINT ( 'NONE',  ( 4.999999999999999112, 0.000000000000000000, 0.000000000000000000 ) ) ;
#1558 = CARTESIAN_POINT ( 'NONE',  ( 0.2500000000000002220, 5.204748896376250699E-16, -4.250000000000000000 ) ) ;
#1559 = ORIENTED_EDGE ( 'NONE', *, *, #8748, .F. ) ;
#1560 = EDGE_LOOP ( 'NONE', ( #8739, #10370, #2728, #4669 ) ) ;
#1561 = DIRECTION ( 'NONE',  ( 0.000000000000000000, -1.000000000000000000, 0.000000000000000000 ) ) ;
#1562 =( LENGTH_UNIT ( ) NAMED_UNIT ( * ) SI_UNIT ( .MILLI., .METRE. ) );
#1563 = DIRECTION ( 'NONE',  ( 1.000000000000000000, -0.000000000000000000, -0.000000000000000000 ) ) ;
#1564 = ORIENTED_EDGE ( 'NONE', *, *, #3179, .F. ) ;
#1565 = FACE_OUTER_BOUND ( 'NONE', #2774, .T. ) ;
#1566 = ORIENTED_EDGE ( 'NONE', *, *, #6391, .F. ) ;
#1567 = CARTESIAN_POINT ( 'NONE',  ( 0.000000000000000000, -14.40062958310459251, -8.872489362018340486 ) ) ;
#1568 = AXIS2_PLACEMENT_3D ( 'NONE', #9560, #4985, #5990 ) ;
#1569 = AXIS2_PLACEMENT_3D ( 'NONE', #10691, #10741, #9882 ) ;
#1570 = EDGE_CURVE ( 'NONE', #5745, #2177, #11460, .T. ) ;
#1571 = EDGE_CURVE ( 'NONE', #9332, #4951, #6562, .T. ) ;
#1572 = EDGE_CURVE ( 'NONE', #3551, #4056, #8964, .T. ) ;
#1573 = DIRECTION ( 'NONE',  ( 0.000000000000000000, 1.000000000000000000, 0.000000000000000000 ) ) ;
#1574 = CARTESIAN_POINT ( 'NONE',  ( 0.000000000000000000, -8.872489362018288972, 14.40062958310462271 ) ) ;
#1575 = DIRECTION ( 'NONE',  ( 0.000000000000000000, 0.3826834323650905589, -0.9238795325112864054 ) ) ;
#1576 = DIRECTION ( 'NONE',  ( 0.000000000000000000, 0.000000000000000000, -1.000000000000000000 ) ) ;
#1577 = VECTOR ( 'NONE', #9990, 1000.000000000000000 ) ;
#1578 = CIRCLE ( 'NONE', #8578, 20.24900000002024569 ) ;
#1579 = ORIENTED_EDGE ( 'NONE', *, *, #3540, .T. ) ;
#1580 = DIRECTION ( 'NONE',  ( 0.000000000000000000, 0.000000000000000000, 1.000000000000000000 ) ) ;
#1581 = CARTESIAN_POINT ( 'NONE',  ( 37.00000000000000711, 0.000000000000000000, 0.000000000000000000 ) ) ;
#1582 = ORIENTED_EDGE ( 'NONE', *, *, #11605, .T. ) ;
#1583 = PLANE ( 'NONE',  #9081 ) ;
#1584 = ORIENTED_EDGE ( 'NONE', *, *, #4095, .F. ) ;
#1585 = EDGE_CURVE ( 'NONE', #11456, #3803, #8168, .T. ) ;
#1586 = AXIS2_PLACEMENT_3D ( 'NONE', #6572, #7575, #9517 ) ;
#1587 = FILL_AREA_STYLE_COLOUR ( '', #3986 ) ;
#1588 = PRESENTATION_LAYER_ASSIGNMENT (  '', '', ( #5777 ) ) ;
#1589 = CARTESIAN_POINT ( 'NONE',  ( 26.00000000000000355, 34.64101615137754919, 20.00000000000000711 ) ) ;
#1590 = CARTESIAN_POINT ( 'NONE',  ( 45.00000000000001421, 50.00000000000000711, -38.00000000000000000 ) ) ;
#1591 = DIRECTION ( 'NONE',  ( 1.000000000000000000, -0.000000000000000000, -0.000000000000000000 ) ) ;
#1592 = DIRECTION ( 'NONE',  ( 0.000000000000000000, 0.000000000000000000, 1.000000000000000000 ) ) ;
#1593 = ORIENTED_EDGE ( 'NONE', *, *, #7120, .T. ) ;
#1594 = FACE_OUTER_BOUND ( 'NONE', #8873, .T. ) ;
#1595 = AXIS2_PLACEMENT_3D ( 'NONE', #10905, #11037, #5102 ) ;
#1596 = ORIENTED_EDGE ( 'NONE', *, *, #809, .T. ) ;
#1597 =( LENGTH_UNIT ( ) NAMED_UNIT ( * ) SI_UNIT ( .MILLI., .METRE. ) );
#1598 = SURFACE_STYLE_USAGE ( .BOTH. , #9246 ) ;
#1599 = EDGE_LOOP ( 'NONE', ( #10743, #9182, #3613, #6472 ) ) ;
#1600 = VECTOR ( 'NONE', #9532, 1000.000000000000000 ) ;
#1601 = CARTESIAN_POINT ( 'NONE',  ( -10.00000000000000000, 0.000000000000000000, 0.000000000000000000 ) ) ;
#1602 = EDGE_CURVE ( 'NONE', #9064, #11240, #2549, .T. ) ;
#1603 = CARTESIAN_POINT ( 'NONE',  ( -13.05124837953327344, 0.000000000000000000, -41.99999999999999289 ) ) ;
#1604 = AXIS2_PLACEMENT_3D ( 'NONE', #9480, #11648, #2959 ) ;
#1605 = ORIENTED_EDGE ( 'NONE', *, *, #9074, .T. ) ;
#1606 = DIRECTION ( 'NONE',  ( 0.000000000000000000, -0.8660254037844433705, 0.4999999999999920064 ) ) ;
#1607 = CIRCLE ( 'NONE', #8209, 20.24900000002024925 ) ;
#1608 = VECTOR ( 'NONE', #3129, 1000.000000000000000 ) ;
#1609 = VERTEX_POINT ( 'NONE', #7912 ) ;
#1610 = DIRECTION ( 'NONE',  ( -1.000000000000000000, -0.000000000000000000, -0.000000000000000000 ) ) ;
#1611 = ORIENTED_EDGE ( 'NONE', *, *, #8738, .F. ) ;
#1612 = SURFACE_SIDE_STYLE ('',( #8312 ) ) ;
#1613 = VECTOR ( 'NONE', #4129, 1000.000000000000000 ) ;
#1614 = CARTESIAN_POINT ( 'NONE',  ( 0.000000000000000000, 0.000000000000000000, 0.000000000000000000 ) ) ;
#1615 = PRODUCT_DEFINITION_SHAPE ( 'NONE', 'NONE',  #5170 ) ;
#1616 = CIRCLE ( 'NONE', #3424, 21.00000000002100009 ) ;
#1617 = ORIENTED_EDGE ( 'NONE', *, *, #3552, .F. ) ;
#1618 = DIRECTION ( 'NONE',  ( -1.000000000000000000, -0.000000000000000000, -0.000000000000000000 ) ) ;
#1619 = AXIS2_PLACEMENT_3D ( 'NONE', #1339, #6229, #8116 ) ;
#1620 = DIRECTION ( 'NONE',  ( 1.000000000000000000, 0.000000000000000000, 0.000000000000000000 ) ) ;
#1621 = AXIS2_PLACEMENT_3D ( 'NONE', #10075, #1503, #9432 ) ;
#1622 = AXIS2_PLACEMENT_3D ( 'NONE', #4950, #7720, #6772 ) ;
#1623 = CIRCLE ( 'NONE', #237, 9.600000000009600853 ) ;
#1624 = CIRCLE ( 'NONE', #7229, 7.200000000007203305 ) ;
#1625 = DIRECTION ( 'NONE',  ( -1.000000000000000000, -0.000000000000000000, 0.000000000000000000 ) ) ;
#1626 = CARTESIAN_POINT ( 'NONE',  ( -20.00000000000000000, 44.00000000000001421, 12.50000000000000000 ) ) ;
#1627 = ORIENTED_EDGE ( 'NONE', *, *, #12236, .T. ) ;
#1628 = ORIENTED_EDGE ( 'NONE', *, *, #11881, .F. ) ;
#1629 = EDGE_CURVE ( 'NONE', #1765, #8354, #6857, .T. ) ;
#1630 = DIRECTION ( 'NONE',  ( 1.000000000000000000, 0.000000000000000000, 0.000000000000000000 ) ) ;
#1631 = DIRECTION ( 'NONE',  ( 0.1305261922200524616, 0.9914448613738103822, -0.000000000000000000 ) ) ;
#1632 = ORIENTED_EDGE ( 'NONE', *, *, #9751, .F. ) ;
#1633 = CARTESIAN_POINT ( 'NONE',  ( -0.1920286436967153787, 0.000000000000000000, 0.000000000000000000 ) ) ;
#1634 = EDGE_CURVE ( 'NONE', #6930, #7756, #6913, .T. ) ;
#1635 = ORIENTED_EDGE ( 'NONE', *, *, #10594, .F. ) ;
#1636 = DIRECTION ( 'NONE',  ( -1.000000000000000000, 0.000000000000000000, 0.000000000000000000 ) ) ;
#1637 = AXIS2_PLACEMENT_3D ( 'NONE', #7596, #92, #6914 ) ;
#1638 = AXIS2_PLACEMENT_3D ( 'NONE', #5013, #4081, #7904 ) ;
#1639 = AXIS2_PLACEMENT_3D ( 'NONE', #1955, #4829, #8652 ) ;
#1640 = CIRCLE ( 'NONE', #240, 2.500000000000002220 ) ;
#1641 = FILL_AREA_STYLE ('',( #10201 ) ) ;
#1642 = DIRECTION ( 'NONE',  ( 0.000000000000000000, 0.000000000000000000, -1.000000000000000000 ) ) ;
#1643 = PRODUCT_DEFINITION_FORMATION_WITH_SPECIFIED_SOURCE ( 'ANY', '', #6628, .NOT_KNOWN. ) ;
#1644 = DIRECTION ( 'NONE',  ( -1.000000000000000000, 0.000000000000000000, -0.000000000000000000 ) ) ;
#1645 = DIRECTION ( 'NONE',  ( 1.000000000000000000, -0.000000000000000000, 0.000000000000000000 ) ) ;
#1646 = CIRCLE ( 'NONE', #2240, 27.00000000002699707 ) ;
#1647 = CIRCLE ( 'NONE', #7850, 21.00000000002100009 ) ;
#1648 = ORIENTED_EDGE ( 'NONE', *, *, #6328, .T. ) ;
#1649 = EDGE_CURVE ( 'NONE', #629, #5118, #5088, .T. ) ;
#1650 = CARTESIAN_POINT ( 'NONE',  ( -0.5000000000000000000, -6.429618962271402616, 0.000000000000000000 ) ) ;
#1651 = AXIS2_PLACEMENT_3D ( 'NONE', #7383, #12110, #6376 ) ;
#1652 = FACE_OUTER_BOUND ( 'NONE', #12014, .T. ) ;
#1653 = EDGE_LOOP ( 'NONE', ( #6606, #6052, #8075, #4915 ) ) ;
#1654 = DIRECTION ( 'NONE',  ( -1.000000000000000000, 0.000000000000000000, 0.000000000000000000 ) ) ;
#1655 = UNCERTAINTY_MEASURE_WITH_UNIT (LENGTH_MEASURE( 1.000000000000000082E-05 ), #6454, 'distance_accuracy_value', 'NONE');
#1656 = EDGE_CURVE ( 'NONE', #5033, #7872, #6765, .T. ) ;
#1657 = VERTEX_POINT ( 'NONE', #3156 ) ;
#1658 = EDGE_CURVE ( 'NONE', #4309, #2267, #8104, .T. ) ;
#1659 = AXIS2_PLACEMENT_3D ( 'NONE', #4254, #2260, #4307 ) ;
#1660 = CIRCLE ( 'NONE', #11831, 4.799999999999998934 ) ;
#1661 = CARTESIAN_POINT ( 'NONE',  ( 29.56763832957518545, 0.000000000000000000, -1.500000000000000000 ) ) ;
#1662 = LINE ( 'NONE', #765, #5799 ) ;
#1663 = DIRECTION ( 'NONE',  ( 0.000000000000000000, -1.000000000000000000, 0.000000000000000000 ) ) ;
#1664 = CARTESIAN_POINT ( 'NONE',  ( 42.00000000000000000, -3.185523555419110586, 3.853886308373666747 ) ) ;
#1665 = CARTESIAN_POINT ( 'NONE',  ( 28.99999999999999645, 6.368163355566238354E-16, -36.79999999999999716 ) ) ;
#1666 = ORIENTED_EDGE ( 'NONE', *, *, #1679, .F. ) ;
#1667 = CARTESIAN_POINT ( 'NONE',  ( -1.250000000000000000, -6.429618962271402616, 0.000000000000000000 ) ) ;
#1668 = AXIS2_PLACEMENT_3D ( 'NONE', #9549, #10605, #5045 ) ;
#1669 = ORIENTED_EDGE ( 'NONE', *, *, #7107, .T. ) ;
#1670 = CARTESIAN_POINT ( 'NONE',  ( 17.00000000000000000, 2.789133085058097101E-16, -2.055000000000000160 ) ) ;
#1671 = AXIS2_PLACEMENT_3D ( 'NONE', #4478, #5537, #8300 ) ;
#1672 = EDGE_LOOP ( 'NONE', ( #2756, #9918, #9368, #11098 ) ) ;
#1673 = EDGE_CURVE ( 'NONE', #317, #10112, #11885, .T. ) ;
#1674 = DIRECTION ( 'NONE',  ( -1.000000000000000000, 0.000000000000000000, -0.000000000000000000 ) ) ;
#1675 = ORIENTED_EDGE ( 'NONE', *, *, #11177, .F. ) ;
#1676 = DIRECTION ( 'NONE',  ( -1.000000000000000000, -0.000000000000000000, -0.000000000000000000 ) ) ;
#1677 = COLOUR_RGB ( '',1.000000000000000000, 0.9490196078431372140, 0.9098039215686274384 ) ;
#1678 = EDGE_LOOP ( 'NONE', ( #10121, #11349, #11716, #1582 ) ) ;
#1679 = EDGE_CURVE ( 'NONE', #11493, #5674, #6035, .T. ) ;
#1680 = EDGE_CURVE ( 'NONE', #3401, #3546, #2275, .T. ) ;
#1681 = FACE_OUTER_BOUND ( 'NONE', #85, .T. ) ;
#1682 = ORIENTED_EDGE ( 'NONE', *, *, #5930, .F. ) ;
#1683 = FILL_AREA_STYLE_COLOUR ( '', #8042 ) ;
#1684 = CARTESIAN_POINT ( 'NONE',  ( -36.00100000000000477, 0.000000000000000000, -47.19999999999998863 ) ) ;
#1685 = CIRCLE ( 'NONE', #1482, 7.200000000007202416 ) ;
#1686 = VERTEX_POINT ( 'NONE', #3101 ) ;
#1687 = CARTESIAN_POINT ( 'NONE',  ( 4.999999999999999112, -11.14352537685160982, -19.60720892790264713 ) ) ;
#1688 = DIRECTION ( 'NONE',  ( -0.000000000000000000, -0.000000000000000000, -1.000000000000000000 ) ) ;
#1689 = CARTESIAN_POINT ( 'NONE',  ( 42.00000000000000000, 0.000000000000000000, 0.000000000000000000 ) ) ;
#1690 = DIRECTION ( 'NONE',  ( 0.000000000000000000, 0.000000000000000000, -1.000000000000000000 ) ) ;
#1691 = ORIENTED_EDGE ( 'NONE', *, *, #9470, .F. ) ;
#1692 = VERTEX_POINT ( 'NONE', #2092 ) ;
#1693 = CARTESIAN_POINT ( 'NONE',  ( 5.000000000000002665, 3.306546357697854226E-16, 2.700000000000000622 ) ) ;
#1694 =( NAMED_UNIT ( * ) PLANE_ANGLE_UNIT ( ) SI_UNIT ( $, .RADIAN. ) );
#1695 = CARTESIAN_POINT ( 'NONE',  ( 37.00000000000000711, 4.769696007084728073, 1.500000000000000444 ) ) ;
#1696 = DIRECTION ( 'NONE',  ( 0.000000000000000000, 0.000000000000000000, 1.000000000000000000 ) ) ;
#1697 = ORIENTED_EDGE ( 'NONE', *, *, #7444, .T. ) ;
#1698 = CARTESIAN_POINT ( 'NONE',  ( 37.00000000000000711, 1.456773409934505593E-31, -41.99999999999998579 ) ) ;
#1699 = VECTOR ( 'NONE', #6648, 1000.000000000000000 ) ;
#1700 = SURFACE_STYLE_USAGE ( .BOTH. , #1756 ) ;
#1701 = DIRECTION ( 'NONE',  ( 0.000000000000000000, 0.000000000000000000, 1.000000000000000000 ) ) ;
#1702 = ADVANCED_FACE ( 'NONE', ( #9959 ), #2144, .T. ) ;
#1703 = ORIENTED_EDGE ( 'NONE', *, *, #10738, .F. ) ;
#1704 = DIRECTION ( 'NONE',  ( 0.000000000000000000, 0.8660254037844398178, -0.4999999999999980016 ) ) ;
#1705 = DIRECTION ( 'NONE',  ( 0.000000000000000000, 0.000000000000000000, -1.000000000000000000 ) ) ;
#1706 = ORIENTED_EDGE ( 'NONE', *, *, #9957, .F. ) ;
#1707 = DIRECTION ( 'NONE',  ( -1.000000000000000000, -0.000000000000000000, -0.000000000000000000 ) ) ;
#1708 = DIRECTION ( 'NONE',  ( -1.000000000000000000, 0.000000000000000000, -0.000000000000000000 ) ) ;
#1709 = VERTEX_POINT ( 'NONE', #9858 ) ;
#1710 = FACE_OUTER_BOUND ( 'NONE', #4150, .T. ) ;
#1711 = ORIENTED_EDGE ( 'NONE', *, *, #7878, .F. ) ;
#1712 = EDGE_CURVE ( 'NONE', #11907, #4096, #9726, .T. ) ;
#1713 = DIRECTION ( 'NONE',  ( 1.000000000000000000, 0.000000000000000000, 0.000000000000000000 ) ) ;
#1714 = DIRECTION ( 'NONE',  ( -0.000000000000000000, 1.000000000000000000, -0.000000000000000000 ) ) ;
#1715 = CARTESIAN_POINT ( 'NONE',  ( 4.999999999999999112, 0.000000000000000000, 0.000000000000000000 ) ) ;
#1716 = EDGE_CURVE ( 'NONE', #11929, #9928, #1147, .T. ) ;
#1717 = DIRECTION ( 'NONE',  ( 1.000000000000000000, 0.000000000000000000, 0.000000000000000000 ) ) ;
#1719 = EDGE_CURVE ( 'NONE', #10717, #10090, #7363, .T. ) ;
#1718 = CARTESIAN_POINT ( 'NONE',  ( 4.999999999999999112, 0.000000000000000000, 0.000000000000000000 ) ) ;
#1720 = ORIENTED_EDGE ( 'NONE', *, *, #10614, .F. ) ;
#1721 = ORIENTED_EDGE ( 'NONE', *, *, #7312, .T. ) ;
#1722 = CARTESIAN_POINT ( 'NONE',  ( 5.000000000000000000, 0.000000000000000000, -1.500000000000000000 ) ) ;
#1723 = VERTEX_POINT ( 'NONE', #4268 ) ;
#1724 = DIRECTION ( 'NONE',  ( 0.000000000000000000, 0.000000000000000000, 1.000000000000000000 ) ) ;
#1725 = APPLICATION_PROTOCOL_DEFINITION ( 'draft international standard', 'automotive_design', 1998, #901 ) ;
#1726 = EDGE_LOOP ( 'NONE', ( #10003, #12274, #2963, #3549 ) ) ;
#1727 = CARTESIAN_POINT ( 'NONE',  ( 36.00000000000000711, -4.210917358895616580, -2.303947698310783387 ) ) ;
#1728 = DIRECTION ( 'NONE',  ( -1.000000000000000000, -0.000000000000000000, 0.000000000000000000 ) ) ;
#1729 = ORIENTED_EDGE ( 'NONE', *, *, #7563, .F. ) ;
#1730 = DIRECTION ( 'NONE',  ( 0.000000000000000000, 0.000000000000000000, -1.000000000000000000 ) ) ;
#1731 = EDGE_CURVE ( 'NONE', #6756, #7499, #326, .T. ) ;
#1732 = EDGE_CURVE ( 'NONE', #102, #6266, #4956, .T. ) ;
#1733 = LINE ( 'NONE', #784, #11796 ) ;
#1734 = EDGE_CURVE ( 'NONE', #4584, #4691, #3168, .T. ) ;
#1735 = ORIENTED_EDGE ( 'NONE', *, *, #2971, .F. ) ;
#1736 = DIRECTION ( 'NONE',  ( -1.000000000000000000, -0.000000000000000000, -0.000000000000000000 ) ) ;
#1737 = ORIENTED_EDGE ( 'NONE', *, *, #1743, .T. ) ;
#1738 = SURFACE_SIDE_STYLE ('',( #12351 ) ) ;
#1739 = DIRECTION ( 'NONE',  ( 0.000000000000000000, 0.000000000000000000, -1.000000000000000000 ) ) ;
#1740 = VERTEX_POINT ( 'NONE', #11760 ) ;
#1741 = DIRECTION ( 'NONE',  ( 0.000000000000000000, 0.5000000000000011102, -0.8660254037844380415 ) ) ;
#1742 = EDGE_CURVE ( 'NONE', #8475, #303, #4087, .T. ) ;
#1743 = EDGE_CURVE ( 'NONE', #1449, #10919, #11133, .T. ) ;
#1744 = DIRECTION ( 'NONE',  ( -1.000000000000000000, -0.000000000000000000, -0.000000000000000000 ) ) ;
#1745 = FACE_OUTER_BOUND ( 'NONE', #2647, .T. ) ;
#1746 = CYLINDRICAL_SURFACE ( 'NONE', #3847, 9.600000000009600853 ) ;
#1747 = VERTEX_POINT ( 'NONE', #10142 ) ;
#1748 = ORIENTED_EDGE ( 'NONE', *, *, #4711, .T. ) ;
#1749 = DIRECTION ( 'NONE',  ( -1.000000000000000000, 0.000000000000000000, 0.000000000000000000 ) ) ;
#1750 = PRESENTATION_STYLE_ASSIGNMENT (( #878 ) ) ;
#1751 = DIRECTION ( 'NONE',  ( 0.000000000000000000, 0.000000000000000000, 1.000000000000000000 ) ) ;
#1752 = CARTESIAN_POINT ( 'NONE',  ( 26.00000000000000355, 0.000000000000000000, -41.99999999999999289 ) ) ;
#1753 = ORIENTED_EDGE ( 'NONE', *, *, #5003, .F. ) ;
#1754 = DIRECTION ( 'NONE',  ( 1.000000000000000000, 0.000000000000000000, 0.000000000000000000 ) ) ;
#1755 = EDGE_CURVE ( 'NONE', #5016, #11122, #5367, .T. ) ;
#1756 = SURFACE_SIDE_STYLE ('',( #12186 ) ) ;
#1757 = FACE_OUTER_BOUND ( 'NONE', #989, .T. ) ;
#1758 = ORIENTED_EDGE ( 'NONE', *, *, #10893, .F. ) ;
#1759 = DIRECTION ( 'NONE',  ( 0.000000000000000000, 0.000000000000000000, -1.000000000000000000 ) ) ;
#1760 = CARTESIAN_POINT ( 'NONE',  ( 4.999999999999999112, 0.000000000000000000, 0.000000000000000000 ) ) ;
#1761 = ORIENTED_EDGE ( 'NONE', *, *, #2117, .F. ) ;
#1762 = FACE_OUTER_BOUND ( 'NONE', #6972, .T. ) ;
#1763 = DIRECTION ( 'NONE',  ( 1.000000000000000000, 0.000000000000000000, 0.000000000000000000 ) ) ;
#1764 = AXIS2_PLACEMENT_3D ( 'NONE', #10362, #11432, #58 ) ;
#1765 = VERTEX_POINT ( 'NONE', #1465 ) ;
#1766 = CARTESIAN_POINT ( 'NONE',  ( 0.000000000000000000, 13.09267581720866858, 5.622796541391611669 ) ) ;
#1767 = UNCERTAINTY_MEASURE_WITH_UNIT (LENGTH_MEASURE( 1.000000000000000082E-05 ), #3696, 'distance_accuracy_value', 'NONE');
#1768 = CIRCLE ( 'NONE', #5365, 27.00000000002699707 ) ;
#1769 = ORIENTED_EDGE ( 'NONE', *, *, #3924, .F. ) ;
#1770 = AXIS2_PLACEMENT_3D ( 'NONE', #7783, #8594, #8665 ) ;
#1771 =( NAMED_UNIT ( * ) SI_UNIT ( $, .STERADIAN. ) SOLID_ANGLE_UNIT ( ) );
#1772 = AXIS2_PLACEMENT_3D ( 'NONE', #9424, #7610, #9546 ) ;
#1773 = CARTESIAN_POINT ( 'NONE',  ( 1.500000000000001332, 6.766173565289127388E-16, 5.525000000000000355 ) ) ;
#1774 = CARTESIAN_POINT ( 'NONE',  ( 37.00000000000000711, -4.104405154062230115E-16, -2.224720805914714718E-17 ) ) ;
#1775 = AXIS2_PLACEMENT_3D ( 'NONE', #7553, #2870, #788 ) ;
#1776 = CARTESIAN_POINT ( 'NONE',  ( 36.00000000000000711, 0.000000000000000000, 0.000000000000000000 ) ) ;
#1777 = CARTESIAN_POINT ( 'NONE',  ( -25.00000000000000000, 6.123233995736766282E-16, -5.000000000000000000 ) ) ;
#1778 = ORIENTED_EDGE ( 'NONE', *, *, #1100, .F. ) ;
#1779 = ORIENTED_EDGE ( 'NONE', *, *, #6986, .T. ) ;
#1780 = CARTESIAN_POINT ( 'NONE',  ( 4.999999999999999112, 0.000000000000000000, 0.000000000000000000 ) ) ;
#1781 = ORIENTED_EDGE ( 'NONE', *, *, #11638, .F. ) ;
#1782 = CARTESIAN_POINT ( 'NONE',  ( 4.999999999999999112, -21.74405275335762155, 5.984728032764886407 ) ) ;
#1783 = EDGE_CURVE ( 'NONE', #5264, #6360, #5358, .T. ) ;
#1784 = SHAPE_DEFINITION_REPRESENTATION ( #10198, #8426 ) ;
#1785 = ORIENTED_EDGE ( 'NONE', *, *, #887, .T. ) ;
#1787 = FACE_OUTER_BOUND ( 'NONE', #881, .T. ) ;
#1786 = VECTOR ( 'NONE', #7800, 1000.000000000000000 ) ;
#1788 = AXIS2_PLACEMENT_3D ( 'NONE', #7262, #6361, #9366 ) ;
#1789 = EDGE_CURVE ( 'NONE', #8068, #9485, #9216, .T. ) ;
#1790 = FACE_BOUND ( 'NONE', #2715, .T. ) ;
#1791 = AXIS2_PLACEMENT_3D ( 'NONE', #10153, #1713, #4336 ) ;
#1792 = ORIENTED_EDGE ( 'NONE', *, *, #1712, .F. ) ;
#1793 = ORIENTED_EDGE ( 'NONE', *, *, #9745, .F. ) ;
#1794 = CARTESIAN_POINT ( 'NONE',  ( 4.999999999999999112, -21.74405275335762155, 5.984728032764886407 ) ) ;
#1795 = LINE ( 'NONE', #4305, #6226 ) ;
#1796 = DIRECTION ( 'NONE',  ( 0.000000000000000000, 0.000000000000000000, 1.000000000000000000 ) ) ;
#1797 = CIRCLE ( 'NONE', #10779, 4.000000000000000000 ) ;
#1798 = VERTEX_POINT ( 'NONE', #5516 ) ;
#1799 = DIRECTION ( 'NONE',  ( -1.000000000000000000, 0.000000000000000000, 0.000000000000000000 ) ) ;
#1800 = ORIENTED_EDGE ( 'NONE', *, *, #4057, .T. ) ;
#1801 = EDGE_CURVE ( 'NONE', #10474, #1992, #3521, .T. ) ;
#1802 = DIRECTION ( 'NONE',  ( -0.000000000000000000, 0.000000000000000000, 1.000000000000000000 ) ) ;
#1803 = EDGE_CURVE ( 'NONE', #6404, #10919, #8358, .T. ) ;
#1805 = ORIENTED_EDGE ( 'NONE', *, *, #11513, .T. ) ;
#1804 = EDGE_CURVE ( 'NONE', #1003, #10175, #6281, .T. ) ;
#1806 = DIRECTION ( 'NONE',  ( 1.000000000000000000, -0.000000000000000000, -0.000000000000000000 ) ) ;
#1807 = EDGE_CURVE ( 'NONE', #11522, #11746, #4154, .T. ) ;
#1808 = VECTOR ( 'NONE', #1573, 1000.000000000000000 ) ;
#1809 = DIRECTION ( 'NONE',  ( -1.000000000000000000, 0.000000000000000000, -0.000000000000000000 ) ) ;
#1810 = DIRECTION ( 'NONE',  ( -0.000000000000000000, 1.000000000000000000, 0.000000000000000000 ) ) ;
#1811 = MECHANICAL_DESIGN_GEOMETRIC_PRESENTATION_REPRESENTATION (  '', ( #11968 ), #9212 ) ;
#1812 = ORIENTED_EDGE ( 'NONE', *, *, #2041, .T. ) ;
#1813 = ORIENTED_EDGE ( 'NONE', *, *, #6114, .F. ) ;
#1814 = LINE ( 'NONE', #7453, #11245 ) ;
#1815 = AXIS2_PLACEMENT_3D ( 'NONE', #1894, #9519, #942 ) ;
#1816 = CARTESIAN_POINT ( 'NONE',  ( 42.00000000000000000, 0.000000000000000000, 5.000000000000000000 ) ) ;
#1817 = AXIS2_PLACEMENT_3D ( 'NONE', #2922, #2790, #1929 ) ;
#1818 = CARTESIAN_POINT ( 'NONE',  ( 3.098410542199072637, -7.060458129626440815, 0.000000000000000000 ) ) ;
#1819 = VERTEX_POINT ( 'NONE', #12069 ) ;
#1820 = CYLINDRICAL_SURFACE ( 'NONE', #3843, 5.000000000000000000 ) ;
#1821 = EDGE_CURVE ( 'NONE', #11485, #26, #11199, .T. ) ;
#1822 = AXIS2_PLACEMENT_3D ( 'NONE', #5485, #6599, #10406 ) ;
#1823 = CIRCLE ( 'NONE', #12195, 14.24900000001425049 ) ;
#1824 = VECTOR ( 'NONE', #5652, 1000.000000000000000 ) ;
#1825 = AXIS2_PLACEMENT_3D ( 'NONE', #7929, #9873, #6296 ) ;
#1826 = AXIS2_PLACEMENT_3D ( 'NONE', #4983, #1115, #8885 ) ;
#1827 = DIRECTION ( 'NONE',  ( -1.000000000000000000, -0.000000000000000000, -0.000000000000000000 ) ) ;
#1828 = CYLINDRICAL_SURFACE ( 'NONE', #3, 6.080745460913608902 ) ;
#1829 = ORIENTED_EDGE ( 'NONE', *, *, #2583, .T. ) ;
#1830 = DIRECTION ( 'NONE',  ( 0.000000000000000000, 0.000000000000000000, 1.000000000000000000 ) ) ;
#1831 = DIRECTION ( 'NONE',  ( -1.000000000000000000, 0.000000000000000000, 0.000000000000000000 ) ) ;
#1832 = ORIENTED_EDGE ( 'NONE', *, *, #7750, .T. ) ;
#1833 = CARTESIAN_POINT ( 'NONE',  ( 0.000000000000000000, 26.33508479058320617, 5.955107813822601237 ) ) ;
#1834 = ADVANCED_FACE ( 'NONE', ( #4514 ), #7167, .F. ) ;
#1835 = DIRECTION ( 'NONE',  ( -1.000000000000000000, -0.000000000000000000, -0.000000000000000000 ) ) ;
#1836 = ADVANCED_FACE ( 'NONE', ( #5333 ), #3463, .T. ) ;
#1837 = AXIS2_PLACEMENT_3D ( 'NONE', #8345, #7481, #5662 ) ;
#1838 = ORIENTED_EDGE ( 'NONE', *, *, #396, .T. ) ;
#1839 = DIRECTION ( 'NONE',  ( 0.000000000000000000, 0.000000000000000000, -1.000000000000000000 ) ) ;
#1840 = CIRCLE ( 'NONE', #2837, 7.500000000000000000 ) ;
#1841 = AXIS2_PLACEMENT_3D ( 'NONE', #1030, #7535, #2962 ) ;
#1842 = VERTEX_POINT ( 'NONE', #9101 ) ;
#1843 = CIRCLE ( 'NONE', #11015, 5.000000000000004441 ) ;
#1844 = CARTESIAN_POINT ( 'NONE',  ( 37.00000000000000711, 4.210917358895616580, 2.303947698310782943 ) ) ;
#1845 = COLOUR_RGB ( '',1.000000000000000000, 0.9490196078431372140, 0.9098039215686274384 ) ;
#1846 = AXIS2_PLACEMENT_3D ( 'NONE', #515, #3157, #2458 ) ;
#1847 = VECTOR ( 'NONE', #309, 1000.000000000000000 ) ;
#1848 = CARTESIAN_POINT ( 'NONE',  ( -38.00000000000000000, 0.000000000000000000, 0.000000000000000000 ) ) ;
#1849 = CARTESIAN_POINT ( 'NONE',  ( 2.500000000000000444, -22.83261415639512393, 14.41081992069302053 ) ) ;
#1850 = VECTOR ( 'NONE', #10513, 1000.000000000000000 ) ;
#1851 = CARTESIAN_POINT ( 'NONE',  ( 20.00000000000000000, 40.00000000000001421, 12.50000000000000000 ) ) ;
#1852 = DIRECTION ( 'NONE',  ( 0.000000000000000000, 0.000000000000000000, 1.000000000000000000 ) ) ;
#1853 = ORIENTED_EDGE ( 'NONE', *, *, #1803, .T. ) ;
#1854 = VERTEX_POINT ( 'NONE', #2566 ) ;
#1855 = DIRECTION ( 'NONE',  ( 0.000000000000000000, 0.000000000000000000, 1.000000000000000000 ) ) ;
#1856 = ORIENTED_EDGE ( 'NONE', *, *, #3640, .T. ) ;
#1857 = VERTEX_POINT ( 'NONE', #9153 ) ;
#1858 = PRODUCT_DEFINITION_FORMATION_WITH_SPECIFIED_SOURCE ( 'ANY', '', #3037, .NOT_KNOWN. ) ;
#1859 = CIRCLE ( 'NONE', #1064, 2.700000000000000178 ) ;
#1860 = FACE_OUTER_BOUND ( 'NONE', #8206, .T. ) ;
#1861 = AXIS2_PLACEMENT_3D ( 'NONE', #4094, #10529, #7862 ) ;
#1862 = VECTOR ( 'NONE', #8140, 1000.000000000000000 ) ;
#1863 = CARTESIAN_POINT ( 'NONE',  ( 26.00000000000000355, 0.000000000000000000, 0.000000000000000000 ) ) ;
#1864 = ORIENTED_EDGE ( 'NONE', *, *, #7519, .T. ) ;
#1865 = ORIENTED_EDGE ( 'NONE', *, *, #8072, .T. ) ;
#1866 = CARTESIAN_POINT ( 'NONE',  ( 37.00000000000000711, -4.210917358895617468, -2.303947698310783831 ) ) ;
#1867 = DIRECTION ( 'NONE',  ( 1.000000000000000000, 0.000000000000000000, 0.000000000000000000 ) ) ;
#1868 = DIRECTION ( 'NONE',  ( -1.000000000000000000, -0.000000000000000000, -0.000000000000000000 ) ) ;
#1869 = ADVANCED_FACE ( 'NONE', ( #5394 ), #11081, .F. ) ;
#1870 = VERTEX_POINT ( 'NONE', #10261 ) ;
#1871 = CIRCLE ( 'NONE', #1466, 9.600000000009600853 ) ;
#1872 = DIRECTION ( 'NONE',  ( 0.000000000000000000, 0.000000000000000000, -1.000000000000000000 ) ) ;
#1873 = VERTEX_POINT ( 'NONE', #569 ) ;
#1874 = EDGE_LOOP ( 'NONE', ( #1935, #4316, #491, #959 ) ) ;
#1875 = LINE ( 'NONE', #2799, #2102 ) ;
#1876 = ORIENTED_EDGE ( 'NONE', *, *, #6781, .T. ) ;
#1877 = DIRECTION ( 'NONE',  ( 1.000000000000000000, -0.000000000000000000, -0.000000000000000000 ) ) ;
#1878 = CARTESIAN_POINT ( 'NONE',  ( 36.00000000000000711, 0.000000000000000000, 0.000000000000000000 ) ) ;
#1879 = EDGE_CURVE ( 'NONE', #1455, #10934, #9336, .T. ) ;
#1880 = ADVANCED_FACE ( 'NONE', ( #10029 ), #514, .T. ) ;
#1881 = CARTESIAN_POINT ( 'NONE',  ( 36.00000000000000000, 0.000000000000000000, -41.99999999999999289 ) ) ;
#1882 = DIRECTION ( 'NONE',  ( 1.000000000000000000, 0.000000000000000000, -0.000000000000000000 ) ) ;
#1883 = EDGE_CURVE ( 'NONE', #5118, #2796, #7109, .T. ) ;
#1884 = ORIENTED_EDGE ( 'NONE', *, *, #6691, .F. ) ;
#1885 = ORIENTED_EDGE ( 'NONE', *, *, #9478, .F. ) ;
#1886 = DIRECTION ( 'NONE',  ( 0.000000000000000000, -1.000000000000000000, 0.000000000000000000 ) ) ;
#1887 =( GEOMETRIC_REPRESENTATION_CONTEXT ( 3 ) GLOBAL_UNCERTAINTY_ASSIGNED_CONTEXT ( ( #4523 ) ) GLOBAL_UNIT_ASSIGNED_CONTEXT ( ( #4965, #6678, #5723 ) ) REPRESENTATION_CONTEXT ( 'NONE', 'WORKASPACE' ) );
#1888 = DIRECTION ( 'NONE',  ( -1.000000000000000000, -0.000000000000000000, 0.000000000000000000 ) ) ;
#1889 = LINE ( 'NONE', #810, #1699 ) ;
#1890 = VERTEX_POINT ( 'NONE', #5462 ) ;
#1891 = DIRECTION ( 'NONE',  ( 0.000000000000000000, 0.000000000000000000, -1.000000000000000000 ) ) ;
#1892 = CIRCLE ( 'NONE', #11854, 2.055000000000000160 ) ;
#1893 = CARTESIAN_POINT ( 'NONE',  ( -38.00000000000000000, 0.000000000000000000, 0.000000000000000000 ) ) ;
#1894 = CARTESIAN_POINT ( 'NONE',  ( -10.00000000000000000, 0.000000000000000000, 0.000000000000000000 ) ) ;
#1895 = ADVANCED_FACE ( 'NONE', ( #9281 ), #701, .F. ) ;
#1896 = CARTESIAN_POINT ( 'NONE',  ( 0.1920286436967153787, 7.516269729766880368E-16, -5.525000000000000355 ) ) ;
#1897 = DIRECTION ( 'NONE',  ( 0.000000000000000000, 0.000000000000000000, -1.000000000000000000 ) ) ;
#1898 = ADVANCED_FACE ( 'NONE', ( #9577 ), #5704, .T. ) ;
#1899 = VERTEX_POINT ( 'NONE', #819 ) ;
#1900 = DIRECTION ( 'NONE',  ( 0.000000000000000000, 0.7071067811865486830, -0.7071067811865464625 ) ) ;
#1901 = CARTESIAN_POINT ( 'NONE',  ( 45.00000000000000000, 0.000000000000000000, 0.000000000000000000 ) ) ;
#1902 = ORIENTED_EDGE ( 'NONE', *, *, #8213, .F. ) ;
#1903 = CARTESIAN_POINT ( 'NONE',  ( 4.799999999999999822, 0.000000000000000000, 0.000000000000000000 ) ) ;
#1904 = AXIS2_PLACEMENT_3D ( 'NONE', #5634, #7514, #8704 ) ;
#1905 = VERTEX_POINT ( 'NONE', #4756 ) ;
#1906 = EDGE_CURVE ( 'NONE', #9112, #5098, #8580, .T. ) ;
#1907 = CARTESIAN_POINT ( 'NONE',  ( -2.354826896168714434, -6.962563485461402024, -1.000000000000000000 ) ) ;
#1908 = ADVANCED_FACE ( 'NONE', ( #2 ), #1828, .T. ) ;
#1909 = CARTESIAN_POINT ( 'NONE',  ( 24.00000000000000000, 0.000000000000000000, -41.99999999999999289 ) ) ;
#1910 = PLANE ( 'NONE',  #2966 ) ;
#1911 = AXIS2_PLACEMENT_3D ( 'NONE', #4432, #8079, #8132 ) ;
#1912 = AXIS2_PLACEMENT_3D ( 'NONE', #1574, #10202, #1642 ) ;
#1913 = DIRECTION ( 'NONE',  ( 0.000000000000000000, 0.9238795325112850731, 0.3826834323650938896 ) ) ;
#1914 = CARTESIAN_POINT ( 'NONE',  ( 4.999999999999999112, -5.984728032765115557, 21.74405275335756116 ) ) ;
#1915 = ORIENTED_EDGE ( 'NONE', *, *, #5846, .F. ) ;
#1916 = EDGE_LOOP ( 'NONE', ( #11600, #6853 ) ) ;
#1917 =( LENGTH_UNIT ( ) NAMED_UNIT ( * ) SI_UNIT ( .MILLI., .METRE. ) );
#1918 = ORIENTED_EDGE ( 'NONE', *, *, #4394, .T. ) ;
#1919 = FILL_AREA_STYLE_COLOUR ( '', #7476 ) ;
#1920 = UNCERTAINTY_MEASURE_WITH_UNIT (LENGTH_MEASURE( 1.000000000000000082E-05 ), #4525, 'distance_accuracy_value', 'NONE');
#1921 = APPLICATION_PROTOCOL_DEFINITION ( 'draft international standard', 'automotive_design', 1998, #11116 ) ;
#1922 = ORIENTED_EDGE ( 'NONE', *, *, #6247, .T. ) ;
#1923 = AXIS2_PLACEMENT_3D ( 'NONE', #889, #10569, #10383 ) ;
#1924 = DIRECTION ( 'NONE',  ( 0.000000000000000000, 0.000000000000000000, 1.000000000000000000 ) ) ;
#1925 = FACE_BOUND ( 'NONE', #6583, .T. ) ;
#1926 = VERTEX_POINT ( 'NONE', #4646 ) ;
#1927 = VERTEX_POINT ( 'NONE', #12308 ) ;
#1928 = FACE_OUTER_BOUND ( 'NONE', #6323, .T. ) ;
#1929 = DIRECTION ( 'NONE',  ( 1.000000000000000000, 0.000000000000000000, 0.000000000000000000 ) ) ;
#1930 = FACE_OUTER_BOUND ( 'NONE', #5467, .T. ) ;
#1931 = CARTESIAN_POINT ( 'NONE',  ( 45.00000000000001421, 46.00000000000001421, -38.00000000000000000 ) ) ;
#1932 = ORIENTED_EDGE ( 'NONE', *, *, #3099, .T. ) ;
#1933 = LINE ( 'NONE', #11297, #7377 ) ;
#1934 = VERTEX_POINT ( 'NONE', #6518 ) ;
#1935 = ORIENTED_EDGE ( 'NONE', *, *, #12053, .F. ) ;
#1936 = LINE ( 'NONE', #7695, #2299 ) ;
#1937 = VERTEX_POINT ( 'NONE', #3758 ) ;
#1938 = CARTESIAN_POINT ( 'NONE',  ( -36.00100000000000477, 0.000000000000000000, -41.99999999999999289 ) ) ;
#1939 = FACE_OUTER_BOUND ( 'NONE', #1061, .T. ) ;
#1940 = CARTESIAN_POINT ( 'NONE',  ( 0.4797447997155618316, -0.6000000000000003109, 3.611077595140663288 ) ) ;
#1941 = CARTESIAN_POINT ( 'NONE',  ( 26.00000000000000355, 0.000000000000000000, 6.500000000000000888 ) ) ;
#1942 = ORIENTED_EDGE ( 'NONE', *, *, #6609, .T. ) ;
#1943 = CARTESIAN_POINT ( 'NONE',  ( 0.1481481481481481122, -4.797713218419819903, -1.000000000000000000 ) ) ;
#1944 = SURFACE_STYLE_USAGE ( .BOTH. , #2886 ) ;
#1945 = DIRECTION ( 'NONE',  ( -1.000000000000000000, -0.000000000000000000, -0.000000000000000000 ) ) ;
#1946 = CARTESIAN_POINT ( 'NONE',  ( -1.399999999999998579, 0.000000000000000000, -7.500000000000000000 ) ) ;
#1947 = EDGE_CURVE ( 'NONE', #9611, #7959, #4806, .T. ) ;
#1948 = EDGE_LOOP ( 'NONE', ( #2361, #5191, #7, #1484 ) ) ;
#1949 = DIRECTION ( 'NONE',  ( -1.000000000000000000, -0.000000000000000000, -0.000000000000000000 ) ) ;
#1950 = EDGE_CURVE ( 'NONE', #2088, #863, #7656, .T. ) ;
#1951 = SURFACE_STYLE_FILL_AREA ( #5755 ) ;
#1952 = PLANE ( 'NONE',  #7605 ) ;
#1953 = SHAPE_REPRESENTATION ( 'circlip for shafts normal_din_Circlip DIN 471 - 10 x 1', ( #6056 ), #3638 ) ;
#1954 = DIRECTION ( 'NONE',  ( 0.000000000000000000, -1.000000000000000000, -1.048062100068272767E-14 ) ) ;
#1955 = CARTESIAN_POINT ( 'NONE',  ( -13.05124837953327344, -12.50000000000000000, -24.50000000000000000 ) ) ;
#1956 = ORIENTED_EDGE ( 'NONE', *, *, #3141, .T. ) ;
#1957 = CARTESIAN_POINT ( 'NONE',  ( 4.999999999999999112, 13.85025647830057416, 17.79862902732270413 ) ) ;
#1958 = CARTESIAN_POINT ( 'NONE',  ( 4.999999999999999112, 0.000000000000000000, 0.000000000000000000 ) ) ;
#1959 = ORIENTED_EDGE ( 'NONE', *, *, #1354, .T. ) ;
#1960 = CARTESIAN_POINT ( 'NONE',  ( 1.600000000000000089, 0.000000000000000000, 0.000000000000000000 ) ) ;
#1961 = ADVANCED_FACE ( 'NONE', ( #10318 ), #1952, .F. ) ;
#1962 = ORIENTED_EDGE ( 'NONE', *, *, #8267, .T. ) ;
#1963 = ADVANCED_FACE ( 'NONE', ( #7579 ), #5833, .F. ) ;
#1964 = EDGE_CURVE ( 'NONE', #1870, #4934, #8008, .T. ) ;
#1965 = ADVANCED_FACE ( 'NONE', ( #1757 ), #7518, .T. ) ;
#1966 = DIRECTION ( 'NONE',  ( -1.000000000000000000, -0.000000000000000000, -0.000000000000000000 ) ) ;
#1967 = CARTESIAN_POINT ( 'NONE',  ( 2.399999999999999467, 0.000000000000000000, 0.000000000000000000 ) ) ;
#1968 = CARTESIAN_POINT ( 'NONE',  ( 2.500000000000000000, -1.768423874527823569, 1.021000000000002794 ) ) ;
#1969 = CARTESIAN_POINT ( 'NONE',  ( 4.999999999999997335, 0.000000000000000000, 0.000000000000000000 ) ) ;
#1970 = DIRECTION ( 'NONE',  ( -1.000000000000000000, 0.000000000000000000, 0.000000000000000000 ) ) ;
#1971 = CIRCLE ( 'NONE', #11952, 0.1000000000000002554 ) ;
#1972 = ORIENTED_EDGE ( 'NONE', *, *, #352, .F. ) ;
#1973 = ORIENTED_EDGE ( 'NONE', *, *, #1042, .F. ) ;
#1974 = AXIS2_PLACEMENT_3D ( 'NONE', #6094, #1276, #5963 ) ;
#1975 = VERTEX_POINT ( 'NONE', #10511 ) ;
#1976 = CARTESIAN_POINT ( 'NONE',  ( 2.500000000000000444, 26.33508479058329499, -5.955107813822217544 ) ) ;
#1977 = ADVANCED_FACE ( 'NONE', ( #3895 ), #8410, .T. ) ;
#1978 = ORIENTED_EDGE ( 'NONE', *, *, #9201, .T. ) ;
#1979 = AXIS2_PLACEMENT_3D ( 'NONE', #6752, #1062, #11302 ) ;
#1980 = VECTOR ( 'NONE', #872, 1000.000000000000000 ) ;
#1981 = VERTEX_POINT ( 'NONE', #11261 ) ;
#1982 = ORIENTED_EDGE ( 'NONE', *, *, #4773, .T. ) ;
#1983 = CARTESIAN_POINT ( 'NONE',  ( 0.000000000000000000, 0.5192545390863916310, -1.000000000000000000 ) ) ;
#1984 = DIRECTION ( 'NONE',  ( -1.000000000000000000, 0.000000000000000000, 0.000000000000000000 ) ) ;
#1985 = DIRECTION ( 'NONE',  ( -1.000000000000000000, -0.000000000000000000, -0.000000000000000000 ) ) ;
#1986 = CARTESIAN_POINT ( 'NONE',  ( 4.999999999999999112, 21.74405275335758247, 5.984728032765037398 ) ) ;
#1987 = ORIENTED_EDGE ( 'NONE', *, *, #12032, .T. ) ;
#1988 = CARTESIAN_POINT ( 'NONE',  ( 25.00000000000000000, 0.000000000000000000, 0.000000000000000000 ) ) ;
#1989 = ORIENTED_EDGE ( 'NONE', *, *, #8647, .T. ) ;
#1990 = CIRCLE ( 'NONE', #5776, 7.200000000007203305 ) ;
#1991 = ADVANCED_FACE ( 'NONE', ( #12253 ), #2697, .T. ) ;
#1992 = VERTEX_POINT ( 'NONE', #2752 ) ;
#1993=STYLED_ITEM('',(#12405),#280);
#1994 = DIRECTION ( 'NONE',  ( 1.000000000000000000, 0.000000000000000000, 0.000000000000000000 ) ) ;
#1995 = ORIENTED_EDGE ( 'NONE', *, *, #7120, .F. ) ;
#1996 = DIRECTION ( 'NONE',  ( 0.000000000000000000, 0.000000000000000000, 1.000000000000000000 ) ) ;
#1997 = AXIS2_PLACEMENT_3D ( 'NONE', #7585, #7663, #3835 ) ;
#1998 = VECTOR ( 'NONE', #1949, 1000.000000000000000 ) ;
#1999 = DIRECTION ( 'NONE',  ( 1.000000000000000000, 0.000000000000000000, 0.000000000000000000 ) ) ;
#2000 = AXIS2_PLACEMENT_3D ( 'NONE', #4303, #2497, #1501 ) ;
#2001 = FACE_OUTER_BOUND ( 'NONE', #2830, .T. ) ;
#2002 = DIRECTION ( 'NONE',  ( 0.000000000000000000, 8.881784197001252323E-15, 1.000000000000000000 ) ) ;
#2003 = EDGE_LOOP ( 'NONE', ( #4948, #9737, #3646, #8879 ) ) ;
#2004 = DIRECTION ( 'NONE',  ( -1.000000000000000000, 0.000000000000000000, -0.000000000000000000 ) ) ;
#2005 = SURFACE_STYLE_FILL_AREA ( #10559 ) ;
#2006 = CARTESIAN_POINT ( 'NONE',  ( 76.00000000000000000, 46.00000000000001421, -41.99999999999999289 ) ) ;
#2007 = AXIS2_PLACEMENT_3D ( 'NONE', #838, #4402, #7531 ) ;
#2008 = CARTESIAN_POINT ( 'NONE',  ( -20.00000000000000000, 40.00000000000000711, 12.50000000000000000 ) ) ;
#2009 = ORIENTED_EDGE ( 'NONE', *, *, #8027, .T. ) ;
#2010 = FACE_OUTER_BOUND ( 'NONE', #6120, .T. ) ;
#2011 = AXIS2_PLACEMENT_3D ( 'NONE', #4987, #8747, #65 ) ;
#2012 = MECHANICAL_DESIGN_GEOMETRIC_PRESENTATION_REPRESENTATION (  '', ( #3009 ), #5200 ) ;
#2013 = DIRECTION ( 'NONE',  ( -1.000000000000000000, -0.000000000000000000, -0.000000000000000000 ) ) ;
#2014 = ADVANCED_FACE ( 'NONE', ( #4702 ), #10454, .T. ) ;
#2015 = AXIS2_PLACEMENT_3D ( 'NONE', #4944, #11557, #3087 ) ;
#2016 = AXIS2_PLACEMENT_3D ( 'NONE', #6308, #5360, #1606 ) ;
#2017 = DIRECTION ( 'NONE',  ( -1.000000000000000000, -0.000000000000000000, -0.000000000000000000 ) ) ;
#2018 = PLANE ( 'NONE',  #4439 ) ;
#2019 = ORIENTED_EDGE ( 'NONE', *, *, #3045, .F. ) ;
#2020 = ADVANCED_FACE ( 'NONE', ( #10755 ), #4074, .F. ) ;
#2021 = DIRECTION ( 'NONE',  ( -1.000000000000000000, 0.000000000000000000, 0.000000000000000000 ) ) ;
#2022 = DIRECTION ( 'NONE',  ( 0.000000000000000000, 0.000000000000000000, 1.000000000000000000 ) ) ;
#2023 = EDGE_LOOP ( 'NONE', ( #10040, #3063, #10805 ) ) ;
#2024 = CARTESIAN_POINT ( 'NONE',  ( -3.309651814758565180, -5.455921364805393026, 0.000000000000000000 ) ) ;
#2025 = UNCERTAINTY_MEASURE_WITH_UNIT (LENGTH_MEASURE( 1.000000000000000082E-05 ), #359, 'distance_accuracy_value', 'NONE');
#2026 = ORIENTED_EDGE ( 'NONE', *, *, #12054, .F. ) ;
#2027 = AXIS2_PLACEMENT_3D ( 'NONE', #9288, #9473, #6341 ) ;
#2028 = AXIS2_PLACEMENT_3D ( 'NONE', #851, #7426, #5491 ) ;
#2029 = LINE ( 'NONE', #2091, #4399 ) ;
#2030 = CARTESIAN_POINT ( 'NONE',  ( -1.400000000000001910, 0.000000000000000000, -5.000000000000000000 ) ) ;
#2031 = EDGE_CURVE ( 'NONE', #10266, #214, #10881, .T. ) ;
#2032 = CARTESIAN_POINT ( 'NONE',  ( 1.400000000000000133, 6.245698675651501825E-16, 5.100000000000000533 ) ) ;
#2033 = DIRECTION ( 'NONE',  ( 0.000000000000000000, 0.000000000000000000, -1.000000000000000000 ) ) ;
#2034 = VECTOR ( 'NONE', #3055, 1000.000000000000000 ) ;
#2035 = AXIS2_PLACEMENT_3D ( 'NONE', #1901, #319, #4136 ) ;
#2036 = ORIENTED_EDGE ( 'NONE', *, *, #9936, .T. ) ;
#2038 = ORIENTED_EDGE ( 'NONE', *, *, #916, .T. ) ;
#2037 = EDGE_CURVE ( 'NONE', #4908, #7756, #8709, .T. ) ;
#2039 = VECTOR ( 'NONE', #389, 1000.000000000000000 ) ;
#2040 = AXIS2_PLACEMENT_3D ( 'NONE', #7493, #1924, #5911 ) ;
#2041 = EDGE_CURVE ( 'NONE', #5044, #4391, #6818, .T. ) ;
#2042 = ORIENTED_EDGE ( 'NONE', *, *, #11893, .F. ) ;
#2043 = PLANE ( 'NONE',  #11253 ) ;
#2044 = ORIENTED_EDGE ( 'NONE', *, *, #10522, .F. ) ;
#2045 =( GEOMETRIC_REPRESENTATION_CONTEXT ( 3 ) GLOBAL_UNCERTAINTY_ASSIGNED_CONTEXT ( ( #897 ) ) GLOBAL_UNIT_ASSIGNED_CONTEXT ( ( #10067, #6256, #11111 ) ) REPRESENTATION_CONTEXT ( 'NONE', 'WORKASPACE' ) );
#2046 = VECTOR ( 'NONE', #1148, 1000.000000000000000 ) ;
#2047 = CIRCLE ( 'NONE', #5042, 5.100000000000000533 ) ;
#2048 = EDGE_LOOP ( 'NONE', ( #3542, #1377 ) ) ;
#2049 = VERTEX_POINT ( 'NONE', #9714 ) ;
#2050 = CARTESIAN_POINT ( 'NONE',  ( 1.600000000000000089, 0.000000000000000000, 2.700000000000000178 ) ) ;
#2051 = LINE ( 'NONE', #5869, #7213 ) ;
#2052 = DIRECTION ( 'NONE',  ( -1.000000000000000000, -0.000000000000000000, -0.000000000000000000 ) ) ;
#2053 = DIRECTION ( 'NONE',  ( 1.000000000000000000, -0.000000000000000000, -0.000000000000000000 ) ) ;
#2054 = ORIENTED_EDGE ( 'NONE', *, *, #11677, .T. ) ;
#2055 = DIRECTION ( 'NONE',  ( 0.000000000000000000, 0.000000000000000000, 1.000000000000000000 ) ) ;
#2056 = DIRECTION ( 'NONE',  ( 1.000000000000000000, -0.000000000000000000, -0.000000000000000000 ) ) ;
#2057 = ORIENTED_EDGE ( 'NONE', *, *, #2972, .F. ) ;
#2058 = AXIS2_PLACEMENT_3D ( 'NONE', #10015, #4559, #6321 ) ;
#2059 = EDGE_LOOP ( 'NONE', ( #4091, #10923 ) ) ;
#2060 = DIRECTION ( 'NONE',  ( -1.000000000000000000, 0.000000000000000000, 0.000000000000000000 ) ) ;
#2061 = VERTEX_POINT ( 'NONE', #2310 ) ;
#2062 = DIRECTION ( 'NONE',  ( 1.000000000000000000, 0.000000000000000000, -0.000000000000000000 ) ) ;
#2063 = VECTOR ( 'NONE', #262, 1000.000000000000000 ) ;
#2064 = CARTESIAN_POINT ( 'NONE',  ( 29.56763832957518545, 6.799999999999998046, 1.500000000000000000 ) ) ;
#2065 = EDGE_CURVE ( 'NONE', #6664, #11679, #2601, .T. ) ;
#2066 = CIRCLE ( 'NONE', #9659, 9.600000000009600853 ) ;
#2067 = ADVANCED_FACE ( 'NONE', ( #7767 ), #10646, .F. ) ;
#2068 = ORIENTED_EDGE ( 'NONE', *, *, #6778, .F. ) ;
#2069 = CARTESIAN_POINT ( 'NONE',  ( -38.00000000000000000, 0.000000000000000000, 0.000000000000000000 ) ) ;
#2070 = CARTESIAN_POINT ( 'NONE',  ( -0.1481481481481481122, -4.797713218419819903, 0.000000000000000000 ) ) ;
#2071 = EDGE_LOOP ( 'NONE', ( #2454, #7760, #5751, #1995 ) ) ;
#2072 = CARTESIAN_POINT ( 'NONE',  ( 4.999999999999999112, -20.18872947935930284, -1.561154383803435408 ) ) ;
#2073 = CYLINDRICAL_SURFACE ( 'NONE', #12012, 7.500000000000000888 ) ;
#2074 = LINE ( 'NONE', #10747, #2096 ) ;
#2075 = CIRCLE ( 'NONE', #5670, 6.000000000000005329 ) ;
#2076 = VERTEX_POINT ( 'NONE', #1260 ) ;
#2077 = DIRECTION ( 'NONE',  ( 1.000000000000000000, 0.000000000000000000, 0.000000000000000000 ) ) ;
#2078 = DIRECTION ( 'NONE',  ( -1.000000000000000000, 0.000000000000000000, 0.000000000000000000 ) ) ;
#2079 = CARTESIAN_POINT ( 'NONE',  ( -3.309651814758565180, -5.455921364805393026, 0.000000000000000000 ) ) ;
#2080 = MECHANICAL_DESIGN_GEOMETRIC_PRESENTATION_REPRESENTATION (  '', ( #3887 ), #10866 ) ;
#2081 = DIRECTION ( 'NONE',  ( 1.000000000000000000, -0.000000000000000000, -0.000000000000000000 ) ) ;
#2082 = CARTESIAN_POINT ( 'NONE',  ( -36.00000000000000711, -9.184850993605149917E-16, 7.500000000000000888 ) ) ;
#2083 = ORIENTED_EDGE ( 'NONE', *, *, #7345, .T. ) ;
#2084 = DIRECTION ( 'NONE',  ( -1.000000000000000000, 0.000000000000000000, 0.000000000000000000 ) ) ;
#2085 = CYLINDRICAL_SURFACE ( 'NONE', #4823, 5.199999999999996625 ) ;
#2086 = ORIENTED_EDGE ( 'NONE', *, *, #1023, .F. ) ;
#2087 = CARTESIAN_POINT ( 'NONE',  ( 0.000000000000000000, 1.561154383803505796, -20.18872947935929574 ) ) ;
#2088 = VERTEX_POINT ( 'NONE', #5127 ) ;
#2089 = AXIS2_PLACEMENT_3D ( 'NONE', #2200, #6087, #4262 ) ;
#2090 = EDGE_CURVE ( 'NONE', #10859, #3765, #134, .T. ) ;
#2091 = CARTESIAN_POINT ( 'NONE',  ( 2.500000000000000000, -2.357898499370432610, 3.252606517456513302E-15 ) ) ;
#2092 = CARTESIAN_POINT ( 'NONE',  ( 36.00000000000000711, 0.000000000000000000, -49.49999999999999289 ) ) ;
#2093 = CARTESIAN_POINT ( 'NONE',  ( 4.999999999999999112, 5.622796541391564595, 13.09267581720868989 ) ) ;
#2094 = DIRECTION ( 'NONE',  ( -1.000000000000000000, 0.000000000000000000, 0.000000000000000000 ) ) ;
#2095 = ORIENTED_EDGE ( 'NONE', *, *, #3826, .F. ) ;
#2096 = VECTOR ( 'NONE', #3191, 1000.000000000000000 ) ;
#2097 = VERTEX_POINT ( 'NONE', #5007 ) ;
#2098 = CARTESIAN_POINT ( 'NONE',  ( 0.000000000000000000, -13.85025647830044271, -17.79862902732279650 ) ) ;
#2099 = ORIENTED_EDGE ( 'NONE', *, *, #10349, .T. ) ;
#2100 = EDGE_CURVE ( 'NONE', #1305, #9964, #11742, .T. ) ;
#2101 = EDGE_CURVE ( 'NONE', #3487, #7536, #3412, .T. ) ;
#2102 = VECTOR ( 'NONE', #9558, 1000.000000000000000 ) ;
#2103 = DIRECTION ( 'NONE',  ( -0.000000000000000000, -1.000000000000000000, -0.000000000000000000 ) ) ;
#2104 = ORIENTED_EDGE ( 'NONE', *, *, #10760, .T. ) ;
#2105 = CARTESIAN_POINT ( 'NONE',  ( 4.999999999999999112, -15.22291137398932470, 14.46592441914959082 ) ) ;
#2106 = DIRECTION ( 'NONE',  ( 0.000000000000000000, 0.000000000000000000, -1.000000000000000000 ) ) ;
#2107 = CARTESIAN_POINT ( 'NONE',  ( 0.000000000000000000, 0.000000000000000000, 0.000000000000000000 ) ) ;
#2108 = FACE_OUTER_BOUND ( 'NONE', #4777, .T. ) ;
#2109 = ORIENTED_EDGE ( 'NONE', *, *, #10098, .T. ) ;
#2110 = CARTESIAN_POINT ( 'NONE',  ( 4.999999999999999112, 0.000000000000000000, 0.000000000000000000 ) ) ;
#2111 = ORIENTED_EDGE ( 'NONE', *, *, #2100, .F. ) ;
#2112 = ORIENTED_EDGE ( 'NONE', *, *, #7381, .T. ) ;
#2113 = DIRECTION ( 'NONE',  ( 0.000000000000000000, 0.000000000000000000, 1.000000000000000000 ) ) ;
#2114 = VERTEX_POINT ( 'NONE', #4185 ) ;
#2115 = CARTESIAN_POINT ( 'NONE',  ( 4.999999999999999112, -14.40062958310471686, 8.872489362018137982 ) ) ;
#2116 = EDGE_CURVE ( 'NONE', #11746, #12042, #1133, .T. ) ;
#2117 = EDGE_CURVE ( 'NONE', #1320, #10764, #7211, .T. ) ;
#2118 = EDGE_CURVE ( 'NONE', #10544, #12146, #1607, .T. ) ;
#2119 = CARTESIAN_POINT ( 'NONE',  ( 46.00000000000000000, 1.456773409934505593E-31, -41.99999999999998579 ) ) ;
#2120 = ORIENTED_EDGE ( 'NONE', *, *, #9829, .F. ) ;
#2121 = CARTESIAN_POINT ( 'NONE',  ( 4.999999999999999112, -15.37949036966221072, 13.17168466712922914 ) ) ;
#2122 = CARTESIAN_POINT ( 'NONE',  ( -19.99999999999999645, 0.000000000000000000, 12.50000000000000000 ) ) ;
#2123 = ORIENTED_EDGE ( 'NONE', *, *, #8447, .T. ) ;
#2124 = CARTESIAN_POINT ( 'NONE',  ( 4.999999999999999112, 26.60936692326690434, 4.576198416197341245 ) ) ;
#2125 =( NAMED_UNIT ( * ) PLANE_ANGLE_UNIT ( ) SI_UNIT ( $, .RADIAN. ) );
#2126 = LINE ( 'NONE', #5748, #11229 ) ;
#2127 = LINE ( 'NONE', #3998, #2490 ) ;
#2128 = EDGE_CURVE ( 'NONE', #3878, #12234, #6840, .T. ) ;
#2129 = ORIENTED_EDGE ( 'NONE', *, *, #1571, .F. ) ;
#2130 = DIRECTION ( 'NONE',  ( -1.000000000000000000, 0.000000000000000000, -0.000000000000000000 ) ) ;
#2131 = EDGE_CURVE ( 'NONE', #7392, #1890, #2203, .T. ) ;
#2132 = DIRECTION ( 'NONE',  ( 1.000000000000000000, 0.000000000000000000, 0.000000000000000000 ) ) ;
#2133 = DIRECTION ( 'NONE',  ( -1.000000000000000000, 0.000000000000000000, 0.000000000000000000 ) ) ;
#2134 = CARTESIAN_POINT ( 'NONE',  ( 0.000000000000000000, -17.79862902732255137, -13.85025647830076245 ) ) ;
#2135 = ORIENTED_EDGE ( 'NONE', *, *, #3047, .F. ) ;
#2136 = DIRECTION ( 'NONE',  ( 1.000000000000000000, 0.000000000000000000, 0.000000000000000000 ) ) ;
#2137 = CARTESIAN_POINT ( 'NONE',  ( 20.00000000000000000, 44.00000000000002132, 12.50000000000000000 ) ) ;
#2138 = ORIENTED_EDGE ( 'NONE', *, *, #4239, .T. ) ;
#2139 = CYLINDRICAL_SURFACE ( 'NONE', #2089, 4.799999999999998934 ) ;
#2140 = EDGE_CURVE ( 'NONE', #1975, #825, #8952, .T. ) ;
#2141 = ORIENTED_EDGE ( 'NONE', *, *, #8087, .T. ) ;
#2142 = CARTESIAN_POINT ( 'NONE',  ( 2.499999999999999556, -4.576198416197437169, 26.60936692326689013 ) ) ;
#2143 = DIRECTION ( 'NONE',  ( 0.000000000000000000, 0.000000000000000000, 1.000000000000000000 ) ) ;
#2144 = CYLINDRICAL_SURFACE ( 'NONE', #7764, 27.00000000002699707 ) ;
#2145 = FACE_OUTER_BOUND ( 'NONE', #3394, .T. ) ;
#2146 = DIRECTION ( 'NONE',  ( 0.000000000000000000, 0.7071067811865437980, 0.7071067811865512365 ) ) ;
#2147 = VERTEX_POINT ( 'NONE', #9768 ) ;
#2148 = CARTESIAN_POINT ( 'NONE',  ( 37.00000000000000711, 1.456773409934505593E-31, -41.99999999999998579 ) ) ;
#2149 = ORIENTED_EDGE ( 'NONE', *, *, #5760, .F. ) ;
#2150 = SHAPE_DEFINITION_REPRESENTATION ( #8046, #7217 ) ;
#2151 = VERTEX_POINT ( 'NONE', #5073 ) ;
#2152 = CARTESIAN_POINT ( 'NONE',  ( 4.999999999999999112, 0.000000000000000000, 0.000000000000000000 ) ) ;
#2153 = ORIENTED_EDGE ( 'NONE', *, *, #147, .F. ) ;
#2154 = DIRECTION ( 'NONE',  ( -1.000000000000000000, 0.000000000000000000, 0.000000000000000000 ) ) ;
#2155 = CARTESIAN_POINT ( 'NONE',  ( -20.00000000000000000, 44.00000000000001421, 12.50000000000000000 ) ) ;
#2156 = FACE_OUTER_BOUND ( 'NONE', #3853, .T. ) ;
#2157 = FACE_OUTER_BOUND ( 'NONE', #6571, .T. ) ;
#2158 = EDGE_CURVE ( 'NONE', #3672, #11750, #3144, .T. ) ;
#2159 = ORIENTED_EDGE ( 'NONE', *, *, #4246, .T. ) ;
#2160 = ORIENTED_EDGE ( 'NONE', *, *, #11856, .F. ) ;
#2161 = ADVANCED_FACE ( 'NONE', ( #7013 ), #8018, .T. ) ;
#2162 = ORIENTED_EDGE ( 'NONE', *, *, #8767, .T. ) ;
#2164 = CARTESIAN_POINT ( 'NONE',  ( 4.999999999999999112, -14.40062958310459251, -1.672489362011137404 ) ) ;
#2163 = AXIS2_PLACEMENT_3D ( 'NONE', #7632, #7560, #12296 ) ;
#2165 = AXIS2_PLACEMENT_3D ( 'NONE', #9508, #178, #4745 ) ;
#2166 = ORIENTED_EDGE ( 'NONE', *, *, #2958, .T. ) ;
#2167 = CARTESIAN_POINT ( 'NONE',  ( 0.2499999999999966416, -8.096141056083448362, 0.000000000000000000 ) ) ;
#2168 = VECTOR ( 'NONE', #5203, 1000.000000000000000 ) ;
#2169 = DIRECTION ( 'NONE',  ( 0.000000000000000000, -0.5000000000000071054, 0.8660254037844345998 ) ) ;
#2170 = AXIS2_PLACEMENT_3D ( 'NONE', #6400, #9341, #5469 ) ;
#2171 = APPLICATION_CONTEXT ( 'automotive_design' ) ;
#2172 = VECTOR ( 'NONE', #862, 1000.000000000000000 ) ;
#2173 = ADVANCED_FACE ( 'NONE', ( #11347, #10011 ), #2366, .T. ) ;
#2174 = ORIENTED_EDGE ( 'NONE', *, *, #4924, .F. ) ;
#2175 = CARTESIAN_POINT ( 'NONE',  ( 4.999999999999999112, -14.40062958310459251, -8.872489362018340486 ) ) ;
#2176 = CYLINDRICAL_SURFACE ( 'NONE', #2869, 0.7500000000000000000 ) ;
#2177 = VERTEX_POINT ( 'NONE', #10999 ) ;
#2178 = FILL_AREA_STYLE ('',( #11684 ) ) ;
#2179 = ADVANCED_FACE ( 'NONE', ( #8194, #3447 ), #9138, .T. ) ;
#2180 =( NAMED_UNIT ( * ) SI_UNIT ( $, .STERADIAN. ) SOLID_ANGLE_UNIT ( ) );
#2181 = CARTESIAN_POINT ( 'NONE',  ( 17.00000000000000000, 0.000000000000000000, 0.000000000000000000 ) ) ;
#2182 = ADVANCED_FACE ( 'NONE', ( #10930 ), #4253, .F. ) ;
#2183 = EDGE_CURVE ( 'NONE', #2572, #866, #5187, .T. ) ;
#2184 = DIRECTION ( 'NONE',  ( 4.770489558936236458E-18, 1.000000000000000000, 0.000000000000000000 ) ) ;
#2185 = EDGE_LOOP ( 'NONE', ( #1918, #10168 ) ) ;
#2186 = DIRECTION ( 'NONE',  ( 1.000000000000000000, -0.000000000000000000, -0.000000000000000000 ) ) ;
#2187 = AXIS2_PLACEMENT_3D ( 'NONE', #1084, #9658, #2831 ) ;
#2188 = AXIS2_PLACEMENT_3D ( 'NONE', #1551, #10178, #8372 ) ;
#2189 = CIRCLE ( 'NONE', #7187, 21.00000000002100009 ) ;
#2190 = LINE ( 'NONE', #6129, #10988 ) ;
#2191 = DIRECTION ( 'NONE',  ( 0.000000000000000000, 0.000000000000000000, -1.000000000000000000 ) ) ;
#2192 = LINE ( 'NONE', #3272, #1464 ) ;
#2193 = CARTESIAN_POINT ( 'NONE',  ( 0.000000000000000000, 20.13931372320397273, -5.950465759858654557 ) ) ;
#2194 = AXIS2_PLACEMENT_3D ( 'NONE', #9870, #11896, #6048 ) ;
#2195 = ORIENTED_EDGE ( 'NONE', *, *, #10853, .F. ) ;
#2196 = DIRECTION ( 'NONE',  ( -1.000000000000000000, 0.000000000000000000, 0.000000000000000000 ) ) ;
#2197 = CARTESIAN_POINT ( 'NONE',  ( 4.999999999999999112, -5.950465759859008941, 20.13931372320386259 ) ) ;
#2198 = PRODUCT_DEFINITION ( 'UNKNOWN', '', #4236, #7024 ) ;
#2199 = ORIENTED_EDGE ( 'NONE', *, *, #5632, .F. ) ;
#2200 = CARTESIAN_POINT ( 'NONE',  ( 43.00000000000000000, 3.903127820947864496E-18, 0.000000000000000000 ) ) ;
#2201 = ORIENTED_EDGE ( 'NONE', *, *, #9315, .T. ) ;
#2202 = DIRECTION ( 'NONE',  ( -1.000000000000000000, 0.000000000000000000, -0.000000000000000000 ) ) ;
#2203 = CIRCLE ( 'NONE', #3012, 5.000000000000000000 ) ;
#2204 = AXIS2_PLACEMENT_3D ( 'NONE', #9934, #7123, #9993 ) ;
#2205 = FACE_OUTER_BOUND ( 'NONE', #6021, .T. ) ;
#2206 = CARTESIAN_POINT ( 'NONE',  ( 37.00000000000000711, 4.210917358895617468, 2.303947698310783387 ) ) ;
#2207 = EDGE_CURVE ( 'NONE', #2502, #542, #9204, .T. ) ;
#2208 = EDGE_CURVE ( 'NONE', #8328, #3785, #5317, .T. ) ;
#2209 = DIRECTION ( 'NONE',  ( 0.000000000000000000, 0.000000000000000000, 1.000000000000000000 ) ) ;
#2210 = CARTESIAN_POINT ( 'NONE',  ( 0.000000000000000000, -6.283573709965167176, -19.24938187143303026 ) ) ;
#2211 = ORIENTED_EDGE ( 'NONE', *, *, #8931, .F. ) ;
#2212 = VECTOR ( 'NONE', #7517, 1000.000000000000000 ) ;
#2213 = ORIENTED_EDGE ( 'NONE', *, *, #4563, .T. ) ;
#2214 = PLANE ( 'NONE',  #9879 ) ;
#2215 = AXIS2_PLACEMENT_3D ( 'NONE', #6745, #11531, #7803 ) ;
#2216 = VERTEX_POINT ( 'NONE', #1446 ) ;
#2217 = CIRCLE ( 'NONE', #11790, 0.7499999999999997780 ) ;
#2218 = DIRECTION ( 'NONE',  ( -0.9914448613738102711, -0.1305261922200524338, 0.000000000000000000 ) ) ;
#2219 = AXIS2_PLACEMENT_3D ( 'NONE', #3119, #2052, #8877 ) ;
#2220 = ORIENTED_EDGE ( 'NONE', *, *, #9403, .F. ) ;
#2221 = VECTOR ( 'NONE', #6215, 1000.000000000000000 ) ;
#2222 = DIRECTION ( 'NONE',  ( -1.000000000000000000, -0.000000000000000000, -0.000000000000000000 ) ) ;
#2223 = CARTESIAN_POINT ( 'NONE',  ( 1.095413108702814053, 0.000000000000000000, 0.000000000000000000 ) ) ;
#2224 = CIRCLE ( 'NONE', #7030, 20.24900000002024569 ) ;
#2225 = AXIS2_PLACEMENT_3D ( 'NONE', #6171, #1540, #597 ) ;
#2226 = LINE ( 'NONE', #8117, #10619 ) ;
#2227 = FACE_OUTER_BOUND ( 'NONE', #833, .T. ) ;
#2228 = ORIENTED_EDGE ( 'NONE', *, *, #5422, .T. ) ;
#2229 = ORIENTED_EDGE ( 'NONE', *, *, #6864, .T. ) ;
#2230 = SURFACE_STYLE_USAGE ( .BOTH. , #3124 ) ;
#2231 = ORIENTED_EDGE ( 'NONE', *, *, #9712, .T. ) ;
#2232 =( GEOMETRIC_REPRESENTATION_CONTEXT ( 3 ) GLOBAL_UNCERTAINTY_ASSIGNED_CONTEXT ( ( #1767 ) ) GLOBAL_UNIT_ASSIGNED_CONTEXT ( ( #3696, #10502, #2811 ) ) REPRESENTATION_CONTEXT ( 'NONE', 'WORKASPACE' ) );
#2233 = CIRCLE ( 'NONE', #4642, 0.1000000000000002554 ) ;
#2234 = CYLINDRICAL_SURFACE ( 'NONE', #228, 7.200000000007202416 ) ;
#2235 = PRODUCT_DEFINITION_SHAPE ( 'NONE', 'NONE',  #8707 ) ;
#2236 = AXIS2_PLACEMENT_3D ( 'NONE', #1278, #5090, #9155 ) ;
#2237 = DIRECTION ( 'NONE',  ( 1.000000000000000000, 0.000000000000000000, 0.000000000000000000 ) ) ;
#2238 = DIRECTION ( 'NONE',  ( 0.000000000000000000, 0.000000000000000000, -1.000000000000000000 ) ) ;
#2239 = ADVANCED_FACE ( 'NONE', ( #4679 ), #5261, .T. ) ;
#2240 = AXIS2_PLACEMENT_3D ( 'NONE', #640, #7521, #6397 ) ;
#2241 = EDGE_LOOP ( 'NONE', ( #1761, #9174, #4530, #6960 ) ) ;
#2242 = AXIS2_PLACEMENT_3D ( 'NONE', #11504, #7717, #1897 ) ;
#2243 = CARTESIAN_POINT ( 'NONE',  ( 36.00000000000000711, 0.000000000000000000, -54.50000000000000000 ) ) ;
#2244 = CARTESIAN_POINT ( 'NONE',  ( 4.999999999999999112, 13.85025647830057416, 17.79862902732270413 ) ) ;
#2245 = ORIENTED_EDGE ( 'NONE', *, *, #1634, .T. ) ;
#2246 = CARTESIAN_POINT ( 'NONE',  ( 46.00000000000000000, 1.456773409934505593E-31, -41.99999999999998579 ) ) ;
#2247 = DIRECTION ( 'NONE',  ( 0.000000000000000000, 0.000000000000000000, -1.000000000000000000 ) ) ;
#2248 = CARTESIAN_POINT ( 'NONE',  ( 0.000000000000000000, -16.90755573046745752, 6.716513609244448624 ) ) ;
#2249 = ORIENTED_EDGE ( 'NONE', *, *, #10231, .T. ) ;
#2250 = DIRECTION ( 'NONE',  ( -1.000000000000000000, 0.000000000000000000, 0.000000000000000000 ) ) ;
#2251 = CARTESIAN_POINT ( 'NONE',  ( 4.999999999999999112, -8.035066368449308882, 14.88411597386726193 ) ) ;
#2252 = VECTOR ( 'NONE', #11067, 1000.000000000000000 ) ;
#2253 = EDGE_CURVE ( 'NONE', #1094, #8881, #10596, .T. ) ;
#2254 = AXIS2_PLACEMENT_3D ( 'NONE', #1626, #5448, #9269 ) ;
#2255 = CARTESIAN_POINT ( 'NONE',  ( 2.500000000000000000, 2.357898499370433054, -1.951563910473907981E-15 ) ) ;
#2256 = ADVANCED_FACE ( 'NONE', ( #3737 ), #2792, .T. ) ;
#2257 = ADVANCED_FACE ( 'NONE', ( #12056 ), #9812, .F. ) ;
#2258 = DIRECTION ( 'NONE',  ( 1.000000000000000000, -0.000000000000000000, 0.000000000000000000 ) ) ;
#2259 = DIRECTION ( 'NONE',  ( -1.000000000000000000, -0.000000000000000000, 0.000000000000000000 ) ) ;
#2260 = DIRECTION ( 'NONE',  ( 1.000000000000000000, 0.000000000000000000, 0.000000000000000000 ) ) ;
#2261 = CARTESIAN_POINT ( 'NONE',  ( 1.000000000000000000, -0.5999999999999995337, -3.826895796574397046 ) ) ;
#2262 = ORIENTED_EDGE ( 'NONE', *, *, #11830, .T. ) ;
#2263 = EDGE_LOOP ( 'NONE', ( #11401, #7942, #5233, #986 ) ) ;
#2264 = CARTESIAN_POINT ( 'NONE',  ( -20.63749999999999574, 9.184850993605147944E-16, 7.500000000000000000 ) ) ;
#2265 = CIRCLE ( 'NONE', #5457, 27.00000000002699707 ) ;
#2266 = LINE ( 'NONE', #11006, #9628 ) ;
#2267 = VERTEX_POINT ( 'NONE', #441 ) ;
#2268 = CARTESIAN_POINT ( 'NONE',  ( 1.500000000000001332, 0.000000000000000000, -6.750000000000000000 ) ) ;
#2269 = PRODUCT_DEFINITION_CONTEXT ( 'detailed design', #4100, 'design' ) ;
#2270 = ORIENTED_EDGE ( 'NONE', *, *, #1679, .T. ) ;
#2271 = CYLINDRICAL_SURFACE ( 'NONE', #11210, 20.24900000002024569 ) ;
#2272 = EDGE_CURVE ( 'NONE', #1981, #4621, #6263, .T. ) ;
#2273 = EDGE_CURVE ( 'NONE', #4298, #2396, #12288, .T. ) ;
#2274 = ADVANCED_FACE ( 'NONE', ( #7272 ), #10076, .T. ) ;
#2275 = LINE ( 'NONE', #385, #10551 ) ;
#2276 = CARTESIAN_POINT ( 'NONE',  ( 4.999999999999999112, -14.41081992069292994, -22.83261415639518432 ) ) ;
#2277 = DIRECTION ( 'NONE',  ( -1.000000000000000000, 0.000000000000000000, -0.000000000000000000 ) ) ;
#2278 = ORIENTED_EDGE ( 'NONE', *, *, #1964, .F. ) ;
#2279 = ORIENTED_EDGE ( 'NONE', *, *, #3566, .T. ) ;
#2280 = DIRECTION ( 'NONE',  ( 0.000000000000000000, 0.000000000000000000, -1.000000000000000000 ) ) ;
#2281 = CIRCLE ( 'NONE', #7082, 1.999999999999998224 ) ;
#2282 = ORIENTED_EDGE ( 'NONE', *, *, #8010, .F. ) ;
#2283 = EDGE_CURVE ( 'NONE', #12241, #1609, #11379, .T. ) ;
#2284 = EDGE_CURVE ( 'NONE', #6613, #26, #5406, .T. ) ;
#2285 = DIRECTION ( 'NONE',  ( 0.000000000000000000, 0.7071067811865486830, -0.7071067811865464625 ) ) ;
#2286 = DIRECTION ( 'NONE',  ( -1.000000000000000000, -0.000000000000000000, -0.000000000000000000 ) ) ;
#2287 = DIRECTION ( 'NONE',  ( -1.000000000000000000, 0.000000000000000000, 0.000000000000000000 ) ) ;
#2288 = AXIS2_PLACEMENT_3D ( 'NONE', #7775, #11643, #9901 ) ;
#2289 = DIRECTION ( 'NONE',  ( -1.000000000000000000, -0.000000000000000000, -0.000000000000000000 ) ) ;
#2290 = CYLINDRICAL_SURFACE ( 'NONE', #5213, 14.24900000001425227 ) ;
#2291 = ORIENTED_EDGE ( 'NONE', *, *, #6309, .F. ) ;
#2292 = CARTESIAN_POINT ( 'NONE',  ( 4.999999999999999112, 13.17168466712928598, 15.37949036966216632 ) ) ;
#2293 = ORIENTED_EDGE ( 'NONE', *, *, #11296, .T. ) ;
#2294 = EDGE_LOOP ( 'NONE', ( #10801, #5806, #7018, #9755 ) ) ;
#2295 = CARTESIAN_POINT ( 'NONE',  ( 37.00000000000000711, 0.000000000000000000, 5.000000000000000000 ) ) ;
#2296 = DIRECTION ( 'NONE',  ( -1.000000000000000000, 0.000000000000000000, 0.000000000000000000 ) ) ;
#2297 = FACE_OUTER_BOUND ( 'NONE', #12132, .T. ) ;
#2298 = VERTEX_POINT ( 'NONE', #8617 ) ;
#2299 = VECTOR ( 'NONE', #2930, 1000.000000000000114 ) ;
#2300 = DIRECTION ( 'NONE',  ( 0.000000000000000000, 0.000000000000000000, 1.000000000000000000 ) ) ;
#2301 = VERTEX_POINT ( 'NONE', #11599 ) ;
#2302 =( NAMED_UNIT ( * ) SI_UNIT ( $, .STERADIAN. ) SOLID_ANGLE_UNIT ( ) );
#2303 = LINE ( 'NONE', #1434, #5639 ) ;
#2304 = CYLINDRICAL_SURFACE ( 'NONE', #8108, 20.24900000002024569 ) ;
#2305 = ORIENTED_EDGE ( 'NONE', *, *, #12265, .T. ) ;
#2306 = CARTESIAN_POINT ( 'NONE',  ( 45.00000000000001421, 46.00000000000001421, -46.00000000000000000 ) ) ;
#2307 = VECTOR ( 'NONE', #11500, 1000.000000000000000 ) ;
#2308 = CARTESIAN_POINT ( 'NONE',  ( -1.500000000000001332, 0.000000000000000000, 0.000000000000000000 ) ) ;
#2309 = DIRECTION ( 'NONE',  ( -1.000000000000000000, -0.000000000000000000, -0.000000000000000000 ) ) ;
#2310 = CARTESIAN_POINT ( 'NONE',  ( 4.999999999999999112, 26.33508479058329499, -5.955107813822219320 ) ) ;
#2311 = FACE_BOUND ( 'NONE', #10416, .T. ) ;
#2312 = FACE_OUTER_BOUND ( 'NONE', #2862, .T. ) ;
#2313 = ORIENTED_EDGE ( 'NONE', *, *, #12104, .T. ) ;
#2314 = EDGE_LOOP ( 'NONE', ( #9553, #5667, #6969, #3684 ) ) ;
#2315 = EDGE_CURVE ( 'NONE', #2452, #10319, #7420, .T. ) ;
#2316 = LINE ( 'NONE', #9718, #4372 ) ;
#2317 = CARTESIAN_POINT ( 'NONE',  ( -3.469446951953614189E-15, 66.91287847477919115, 12.50000000000000000 ) ) ;
#2318 = VERTEX_POINT ( 'NONE', #1931 ) ;
#2319 = DIRECTION ( 'NONE',  ( 0.000000000000000000, -1.000000000000000000, 0.000000000000000000 ) ) ;
#2320 = EDGE_CURVE ( 'NONE', #4040, #1069, #1159, .T. ) ;
#2321 = ORIENTED_EDGE ( 'NONE', *, *, #16, .T. ) ;
#2322 = DIRECTION ( 'NONE',  ( -1.000000000000000000, -0.000000000000000000, -0.000000000000000000 ) ) ;
#2323 = FILL_AREA_STYLE ('',( #1208 ) ) ;
#2324 = CARTESIAN_POINT ( 'NONE',  ( -3.098410542199071749, -7.060458129626440815, -1.000000000000000000 ) ) ;
#2325 = LINE ( 'NONE', #5334, #4051 ) ;
#2326 = LINE ( 'NONE', #1390, #2039 ) ;
#2327 = PRODUCT_DEFINITION_SHAPE ( 'NONE', 'NONE',  #12358 ) ;
#2328 = VERTEX_POINT ( 'NONE', #7876 ) ;
#2329 = EDGE_CURVE ( 'NONE', #1083, #10418, #1020, .T. ) ;
#2330 = FACE_OUTER_BOUND ( 'NONE', #11963, .T. ) ;
#2331 = EDGE_LOOP ( 'NONE', ( #10322, #679, #6415, #5369 ) ) ;
#2332 = CARTESIAN_POINT ( 'NONE',  ( 0.000000000000000000, 0.000000000000000000, -1.000000000000000000 ) ) ;
#2333 = EDGE_CURVE ( 'NONE', #8484, #8701, #3056, .T. ) ;
#2334 = EDGE_CURVE ( 'NONE', #1494, #3376, #2866, .T. ) ;
#2335 = ORIENTED_EDGE ( 'NONE', *, *, #1399, .T. ) ;
#2336 = ADVANCED_FACE ( 'NONE', ( #4865 ), #9687, .T. ) ;
#2337 = CARTESIAN_POINT ( 'NONE',  ( 4.999999999999997335, 0.000000000000000000, 0.000000000000000000 ) ) ;
#2338 = CARTESIAN_POINT ( 'NONE',  ( 4.999999999999999112, 8.527191590521233877, -11.41582255376064126 ) ) ;
#2339 = CARTESIAN_POINT ( 'NONE',  ( -1.400000000000000133, 0.000000000000000000, 0.000000000000000000 ) ) ;
#2340 = DIRECTION ( 'NONE',  ( -1.000000000000000000, 0.000000000000000000, 0.000000000000000000 ) ) ;
#2341 = DIRECTION ( 'NONE',  ( 0.000000000000000000, -0.8386705679454229401, -0.5446390350150287496 ) ) ;
#2342 = EDGE_LOOP ( 'NONE', ( #6267, #8605, #1342, #9024, #5916 ) ) ;
#2343 = ADVANCED_FACE ( 'NONE', ( #9619 ), #10485, .T. ) ;
#2344 = DIRECTION ( 'NONE',  ( 1.000000000000000000, 0.000000000000000000, 0.000000000000000000 ) ) ;
#2345 = VERTEX_POINT ( 'NONE', #6804 ) ;
#2346 = DIRECTION ( 'NONE',  ( 1.000000000000000000, 0.000000000000000000, 0.000000000000000000 ) ) ;
#2347 = ORIENTED_EDGE ( 'NONE', *, *, #87, .T. ) ;
#2348 = FACE_OUTER_BOUND ( 'NONE', #9404, .T. ) ;
#2349 = LINE ( 'NONE', #481, #1577 ) ;
#2350 = ORIENTED_EDGE ( 'NONE', *, *, #6782, .F. ) ;
#2351 = DIRECTION ( 'NONE',  ( 1.000000000000000000, 0.000000000000000000, 0.000000000000000000 ) ) ;
#2352 = ORIENTED_EDGE ( 'NONE', *, *, #5484, .F. ) ;
#2353 = EDGE_CURVE ( 'NONE', #5917, #10787, #6630, .T. ) ;
#2354 = ADVANCED_FACE ( 'NONE', ( #3923, #2108 ), #9552, .T. ) ;
#2355 = DIRECTION ( 'NONE',  ( -1.000000000000000000, 0.000000000000000000, 0.000000000000000000 ) ) ;
#2356 = AXIS2_PLACEMENT_3D ( 'NONE', #8746, #11787, #11722 ) ;
#2357 = ORIENTED_EDGE ( 'NONE', *, *, #6887, .T. ) ;
#2358 = LINE ( 'NONE', #10745, #1847 ) ;
#2359 = VECTOR ( 'NONE', #2908, 1000.000000000000000 ) ;
#2360 = CARTESIAN_POINT ( 'NONE',  ( 4.999999999999999112, 0.000000000000000000, 14.24900000001425227 ) ) ;
#2361 = ORIENTED_EDGE ( 'NONE', *, *, #8783, .F. ) ;
#2362 = CARTESIAN_POINT ( 'NONE',  ( 26.00000000000000355, 12.50000000000000000, -41.99999999999999289 ) ) ;
#2363 = VECTOR ( 'NONE', #2021, 1000.000000000000000 ) ;
#2364 = CIRCLE ( 'NONE', #2165, 7.200000000007202416 ) ;
#2365 = PLANE ( 'NONE',  #5005 ) ;
#2366 = PLANE ( 'NONE',  #2407 ) ;
#2367 = DIRECTION ( 'NONE',  ( -1.000000000000000000, 0.000000000000000000, 0.000000000000000000 ) ) ;
#2368 = PLANE ( 'NONE',  #2254 ) ;
#2369 = ORIENTED_EDGE ( 'NONE', *, *, #10422, .T. ) ;
#2370 = ORIENTED_EDGE ( 'NONE', *, *, #3102, .F. ) ;
#2371 = DIRECTION ( 'NONE',  ( -1.000000000000000000, 0.000000000000000000, 0.000000000000000000 ) ) ;
#2372 = CARTESIAN_POINT ( 'NONE',  ( 0.000000000000000000, 0.000000000000000000, 0.000000000000000000 ) ) ;
#2373 = CARTESIAN_POINT ( 'NONE',  ( 42.00000000000000000, 0.000000000000000000, 0.000000000000000000 ) ) ;
#2374 = CIRCLE ( 'NONE', #6382, 14.24900000001425227 ) ;
#2375 = ORIENTED_EDGE ( 'NONE', *, *, #8013, .T. ) ;
#2376 = CYLINDRICAL_SURFACE ( 'NONE', #4688, 27.00000000002699707 ) ;
#2377 = PRODUCT_DEFINITION_CONTEXT ( 'detailed design', #12232, 'design' ) ;
#2378 = VECTOR ( 'NONE', #7623, 1000.000000000000000 ) ;
#2379 = ORIENTED_EDGE ( 'NONE', *, *, #6701, .T. ) ;
#2380 = LINE ( 'NONE', #3154, #9429 ) ;
#2381 = CIRCLE ( 'NONE', #11757, 6.975000000000000533 ) ;
#2382 = ADVANCED_FACE ( 'NONE', ( #4976 ), #230, .T. ) ;
#2383 = CIRCLE ( 'NONE', #7794, 12.49999999999999645 ) ;
#2384 = FILL_AREA_STYLE ('',( #8858 ) ) ;
#2385 = DIRECTION ( 'NONE',  ( -1.000000000000000000, -0.000000000000000000, -0.000000000000000000 ) ) ;
#2386 = CIRCLE ( 'NONE', #5753, 7.500000000000000888 ) ;
#2387 = EDGE_CURVE ( 'NONE', #9031, #31, #5616, .T. ) ;
#2388 = AXIS2_PLACEMENT_3D ( 'NONE', #6318, #1809, #10126 ) ;
#2389 = DIRECTION ( 'NONE',  ( 0.000000000000000000, 0.000000000000000000, 1.000000000000000000 ) ) ;
#2390 = CARTESIAN_POINT ( 'NONE',  ( 2.499999999999999556, 26.33508479058320617, 5.955107813822601237 ) ) ;
#2391 = ORIENTED_EDGE ( 'NONE', *, *, #2517, .T. ) ;
#2392 = CYLINDRICAL_SURFACE ( 'NONE', #5568, 7.500000000000000000 ) ;
#2393 = CARTESIAN_POINT ( 'NONE',  ( 0.000000000000000000, 0.000000000000000000, 6.250000000000000000 ) ) ;
#2394 = ORIENTED_EDGE ( 'NONE', *, *, #8102, .F. ) ;
#2395 =( LENGTH_UNIT ( ) NAMED_UNIT ( * ) SI_UNIT ( .MILLI., .METRE. ) );
#2396 = VERTEX_POINT ( 'NONE', #9741 ) ;
#2397 = VECTOR ( 'NONE', #818, 1000.000000000000000 ) ;
#2398 = VECTOR ( 'NONE', #7063, 1000.000000000000000 ) ;
#2399 = EDGE_CURVE ( 'NONE', #11586, #6059, #3867, .T. ) ;
#2400 = CARTESIAN_POINT ( 'NONE',  ( -15.00000000000000000, 30.00000000000000711, 0.000000000000000000 ) ) ;
#2401 = DIRECTION ( 'NONE',  ( 0.000000000000000000, -1.000000000000000000, 0.000000000000000000 ) ) ;
#2402 = EDGE_CURVE ( 'NONE', #1109, #7442, #5678, .T. ) ;
#2403 = DIRECTION ( 'NONE',  ( 1.000000000000000000, 0.000000000000000000, 0.000000000000000000 ) ) ;
#2405 = EDGE_CURVE ( 'NONE', #12064, #3807, #9823, .T. ) ;
#2404 = CYLINDRICAL_SURFACE ( 'NONE', #8421, 6.975000000000000533 ) ;
#2406 = ORIENTED_EDGE ( 'NONE', *, *, #42, .T. ) ;
#2407 = AXIS2_PLACEMENT_3D ( 'NONE', #1504, #11118, #550 ) ;
#2408 = DIRECTION ( 'NONE',  ( -1.000000000000000000, 0.000000000000000000, 0.000000000000000000 ) ) ;
#2409 = AXIS2_PLACEMENT_3D ( 'NONE', #11970, #6359, #3611 ) ;
#2410 = ORIENTED_EDGE ( 'NONE', *, *, #6368, .F. ) ;
#2411 = DIRECTION ( 'NONE',  ( 1.577229628477151377E-17, -0.5750543479813584602, -0.8181152100210181688 ) ) ;
#2412 = EDGE_LOOP ( 'NONE', ( #5592, #9422, #3936, #5147 ) ) ;
#2413 = LINE ( 'NONE', #9178, #11991 ) ;
#2414 =( REPRESENTATION_RELATIONSHIP ('NONE','NONE', #9709, #11360 ) REPRESENTATION_RELATIONSHIP_WITH_TRANSFORMATION ( #1038 )SHAPE_REPRESENTATION_RELATIONSHIP( ) );
#2415 = DIRECTION ( 'NONE',  ( 0.000000000000000000, 0.000000000000000000, -1.000000000000000000 ) ) ;
#2416 = CIRCLE ( 'NONE', #10209, 4.800000000000000711 ) ;
#2417 = CIRCLE ( 'NONE', #224, 27.00000000002699707 ) ;
#2418 = AXIS2_PLACEMENT_3D ( 'NONE', #977, #921, #47 ) ;
#2419 = CIRCLE ( 'NONE', #2225, 9.600000000009599077 ) ;
#2420 = ORIENTED_EDGE ( 'NONE', *, *, #5139, .F. ) ;
#2421 = DIRECTION ( 'NONE',  ( -1.000000000000000000, -0.000000000000000000, 0.000000000000000000 ) ) ;
#2422 = EDGE_CURVE ( 'NONE', #303, #11981, #4418, .T. ) ;
#2423 = ORIENTED_EDGE ( 'NONE', *, *, #662, .F. ) ;
#2424 = FACE_OUTER_BOUND ( 'NONE', #7547, .T. ) ;
#2425 = AXIS2_PLACEMENT_3D ( 'NONE', #6803, #4864, #11665 ) ;
#2426 = VERTEX_POINT ( 'NONE', #12345 ) ;
#2427 = CIRCLE ( 'NONE', #9427, 9.600000000009597301 ) ;
#2428 = AXIS2_PLACEMENT_3D ( 'NONE', #12067, #3461, #10315 ) ;
#2429 = CYLINDRICAL_SURFACE ( 'NONE', #9502, 7.500000000000000000 ) ;
#2430 = ORIENTED_EDGE ( 'NONE', *, *, #2884, .T. ) ;
#2431 = FACE_OUTER_BOUND ( 'NONE', #8863, .T. ) ;
#2432 = EDGE_CURVE ( 'NONE', #6862, #5581, #14, .T. ) ;
#2433 = EDGE_CURVE ( 'NONE', #7460, #8470, #7618, .T. ) ;
#2434 = VECTOR ( 'NONE', #1591, 1000.000000000000000 ) ;
#2435 = VECTOR ( 'NONE', #8930, 1000.000000000000000 ) ;
#2436 = FACE_OUTER_BOUND ( 'NONE', #12125, .T. ) ;
#2437 = VECTOR ( 'NONE', #12011, 1000.000000000000000 ) ;
#2438 = FACE_OUTER_BOUND ( 'NONE', #9609, .T. ) ;
#2439 = CARTESIAN_POINT ( 'NONE',  ( 4.999999999999997335, 0.000000000000000000, 0.000000000000000000 ) ) ;
#2440 = LINE ( 'NONE', #8318, #2252 ) ;
#2441 = CARTESIAN_POINT ( 'NONE',  ( 36.00000000000000711, 1.456773409934505593E-31, -41.99999999999998579 ) ) ;
#2442 = ORIENTED_EDGE ( 'NONE', *, *, #9009, .T. ) ;
#2443 = ORIENTED_EDGE ( 'NONE', *, *, #2933, .F. ) ;
#2444 = CARTESIAN_POINT ( 'NONE',  ( 0.3700949531097381118, -0.5999999999999994227, -3.517837443070535919 ) ) ;
#2445 = DIRECTION ( 'NONE',  ( 0.000000000000000000, 0.000000000000000000, 1.000000000000000000 ) ) ;
#2446 = AXIS2_PLACEMENT_3D ( 'NONE', #10055, #1486, #535 ) ;
#2447 = CIRCLE ( 'NONE', #6658, 20.24900000002024569 ) ;
#2448 = ORIENTED_EDGE ( 'NONE', *, *, #11359, .F. ) ;
#2449 = DIRECTION ( 'NONE',  ( 0.000000000000000000, 0.000000000000000000, 1.000000000000000000 ) ) ;
#2450 = CIRCLE ( 'NONE', #6624, 5.199999999999996625 ) ;
#2451 = CIRCLE ( 'NONE', #655, 5.000000000000000000 ) ;
#2452 = VERTEX_POINT ( 'NONE', #1341 ) ;
#2453 = CARTESIAN_POINT ( 'NONE',  ( 43.00000000000000000, 3.792354139917828437, 2.942456469932579921 ) ) ;
#2454 = ORIENTED_EDGE ( 'NONE', *, *, #2065, .T. ) ;
#2455 =( NAMED_UNIT ( * ) SI_UNIT ( $, .STERADIAN. ) SOLID_ANGLE_UNIT ( ) );
#2456 = CARTESIAN_POINT ( 'NONE',  ( 29.56763832957518545, 6.799999999999998046, -1.500000000000000000 ) ) ;
#2457 = CIRCLE ( 'NONE', #6260, 7.500000000000000000 ) ;
#2458 = DIRECTION ( 'NONE',  ( 0.000000000000000000, 0.000000000000000000, 1.000000000000000000 ) ) ;
#2459 = DIRECTION ( 'NONE',  ( 0.000000000000000000, 0.000000000000000000, 1.000000000000000000 ) ) ;
#2460 = EDGE_LOOP ( 'NONE', ( #11520, #8365, #3341, #7305 ) ) ;
#2461 = CARTESIAN_POINT ( 'NONE',  ( -13.05124837953327344, 12.50000000000000000, -41.99999999999999289 ) ) ;
#2462 = DIRECTION ( 'NONE',  ( -0.000000000000000000, 1.471414886128461471E-15, 1.000000000000000000 ) ) ;
#2463 = ORIENTED_EDGE ( 'NONE', *, *, #7322, .F. ) ;
#2464 = DIRECTION ( 'NONE',  ( 0.000000000000000000, 0.000000000000000000, -1.000000000000000000 ) ) ;
#2465 = ITEM_DEFINED_TRANSFORMATION ( 'NONE', 'NONE', #11031,  #6056 ) ;
#2466 = EDGE_LOOP ( 'NONE', ( #4188, #1779, #10162, #1499 ) ) ;
#2467 = AXIS2_PLACEMENT_3D ( 'NONE', #11623, #10807, #3079 ) ;
#2468 = FACE_OUTER_BOUND ( 'NONE', #11107, .T. ) ;
#2469 = DIRECTION ( 'NONE',  ( -1.000000000000000000, 0.000000000000000000, 0.000000000000000000 ) ) ;
#2470 = CARTESIAN_POINT ( 'NONE',  ( 4.999999999999999112, -22.37914155802287297, 2.791921004064167544 ) ) ;
#2471 = FACE_BOUND ( 'NONE', #587, .T. ) ;
#2472 = DIRECTION ( 'NONE',  ( 0.000000000000000000, 0.000000000000000000, -1.000000000000000000 ) ) ;
#2473 = EDGE_LOOP ( 'NONE', ( #759, #11121, #3067, #8261 ) ) ;
#2474 = AXIS2_PLACEMENT_3D ( 'NONE', #9604, #32, #99 ) ;
#2475 = CARTESIAN_POINT ( 'NONE',  ( 2.499999999999998668, -14.46592441914954286, -15.22291137398937089 ) ) ;
#2476 = EDGE_LOOP ( 'NONE', ( #2787, #1706, #9471, #3437 ) ) ;
#2477 = ADVANCED_FACE ( 'NONE', ( #3170 ), #6980, .T. ) ;
#2478 =( NAMED_UNIT ( * ) PLANE_ANGLE_UNIT ( ) SI_UNIT ( $, .RADIAN. ) );
#2479 = ORIENTED_EDGE ( 'NONE', *, *, #7267, .F. ) ;
#2480 = DIRECTION ( 'NONE',  ( 0.03086419753086420623, 0.9995235871707959241, -0.000000000000000000 ) ) ;
#2481 = ADVANCED_FACE ( 'NONE', ( #4156 ), #2290, .T. ) ;
#2482 = CARTESIAN_POINT ( 'NONE',  ( 36.00000000000000000, 40.00000000000000711, 20.00000000000001066 ) ) ;
#2483 = VECTOR ( 'NONE', #4656, 1000.000000000000000 ) ;
#2484 = ORIENTED_EDGE ( 'NONE', *, *, #42, .F. ) ;
#2485 = DIRECTION ( 'NONE',  ( 0.000000000000000000, 0.8660254037844363761, 0.5000000000000041078 ) ) ;
#2486 = VERTEX_POINT ( 'NONE', #10786 ) ;
#2487 = DIRECTION ( 'NONE',  ( -1.000000000000000000, 0.000000000000000000, -0.000000000000000000 ) ) ;
#2488 = ORIENTED_EDGE ( 'NONE', *, *, #4269, .T. ) ;
#2489 = EDGE_CURVE ( 'NONE', #7042, #11456, #5158, .T. ) ;
#2490 = VECTOR ( 'NONE', #5178, 1000.000000000000000 ) ;
#2491 = DIRECTION ( 'NONE',  ( 0.000000000000000000, 0.000000000000000000, 1.000000000000000000 ) ) ;
#2492 = ADVANCED_FACE ( 'NONE', ( #1404 ), #2404, .F. ) ;
#2494 = ORIENTED_EDGE ( 'NONE', *, *, #11514, .F. ) ;
#2493 = EDGE_CURVE ( 'NONE', #5118, #2913, #227, .T. ) ;
#2495 = CARTESIAN_POINT ( 'NONE',  ( 2.500000000000000000, -2.357898499370432610, 3.252606517456513302E-15 ) ) ;
#2496 = ADVANCED_FACE ( 'NONE', ( #8170 ), #6110, .T. ) ;
#2497 = DIRECTION ( 'NONE',  ( 0.000000000000000000, 0.000000000000000000, 1.000000000000000000 ) ) ;
#2498 = CIRCLE ( 'NONE', #11680, 7.200000000007200640 ) ;
#2499 = DIRECTION ( 'NONE',  ( 0.000000000000000000, 0.000000000000000000, 1.000000000000000000 ) ) ;
#2500 = DIRECTION ( 'NONE',  ( 0.000000000000000000, 0.6828850436591804574, 0.7305258497456468270 ) ) ;
#2501 = CYLINDRICAL_SURFACE ( 'NONE', #2058, 20.24900000002024569 ) ;
#2502 = VERTEX_POINT ( 'NONE', #8878 ) ;
#2503 = EDGE_LOOP ( 'NONE', ( #1450, #8286, #2352, #8726 ) ) ;
#2504 = DIRECTION ( 'NONE',  ( -1.000000000000000000, 0.000000000000000000, 0.000000000000000000 ) ) ;
#2505 = EDGE_CURVE ( 'NONE', #1094, #7890, #11958, .T. ) ;
#2506 = CARTESIAN_POINT ( 'NONE',  ( 42.00000000000000000, 4.814824860968089633E-32, 0.000000000000000000 ) ) ;
#2507 = ORIENTED_EDGE ( 'NONE', *, *, #9297, .T. ) ;
#2508 = CARTESIAN_POINT ( 'NONE',  ( 51.00000000000000000, 1.444447458290426890E-31, -41.99999999999998579 ) ) ;
#2509 = ORIENTED_EDGE ( 'NONE', *, *, #2353, .F. ) ;
#2510 = DIRECTION ( 'NONE',  ( -1.000000000000000000, 0.000000000000000000, -0.000000000000000000 ) ) ;
#2511 = CARTESIAN_POINT ( 'NONE',  ( 42.00000000000000000, 6.519918414551419517, -39.55446041381592437 ) ) ;
#2512 = CARTESIAN_POINT ( 'NONE',  ( 20.00000000000000000, 44.00000000000002132, -12.50000000000000000 ) ) ;
#2513 = DIRECTION ( 'NONE',  ( 1.000000000000000000, 0.000000000000000000, 0.000000000000000000 ) ) ;
#2514 = DIRECTION ( 'NONE',  ( 0.000000000000000000, 0.000000000000000000, -1.000000000000000000 ) ) ;
#2515 = VERTEX_POINT ( 'NONE', #6161 ) ;
#2516 = CYLINDRICAL_SURFACE ( 'NONE', #5772, 7.200000000007204193 ) ;
#2517 = EDGE_CURVE ( 'NONE', #9474, #644, #610, .T. ) ;
#2518 = CARTESIAN_POINT ( 'NONE',  ( 27.38165010660258503, 5.702959862028875726, -38.29645456189778940 ) ) ;
#2519 = ORIENTED_EDGE ( 'NONE', *, *, #7762, .T. ) ;
#2520 = DIRECTION ( 'NONE',  ( 0.000000000000000000, -1.224646799147353454E-16, 1.000000000000000000 ) ) ;
#2521 = UNCERTAINTY_MEASURE_WITH_UNIT (LENGTH_MEASURE( 1.000000000000000082E-05 ), #1562, 'distance_accuracy_value', 'NONE');
#2522 = EDGE_LOOP ( 'NONE', ( #5996, #6162, #7863, #2245 ) ) ;
#2523 = DIRECTION ( 'NONE',  ( -0.000000000000000000, 0.000000000000000000, 1.000000000000000000 ) ) ;
#2524 = DIRECTION ( 'NONE',  ( 0.000000000000000000, 0.000000000000000000, 1.000000000000000000 ) ) ;
#2525 = CYLINDRICAL_SURFACE ( 'NONE', #10013, 7.000000000000004441 ) ;
#2526 = DIRECTION ( 'NONE',  ( 0.000000000000000000, 1.000000000000000000, 3.491481338843133355E-15 ) ) ;
#2527 = DIRECTION ( 'NONE',  ( 1.000000000000000000, 0.000000000000000000, 0.000000000000000000 ) ) ;
#2528 = EDGE_LOOP ( 'NONE', ( #217, #6881, #10064, #11949 ) ) ;
#2529 = DIRECTION ( 'NONE',  ( 0.000000000000000000, 0.000000000000000000, 1.000000000000000000 ) ) ;
#2530 = ORIENTED_EDGE ( 'NONE', *, *, #6325, .F. ) ;
#2531 = DIRECTION ( 'NONE',  ( -1.000000000000000000, -0.000000000000000000, -0.000000000000000000 ) ) ;
#2532 = VERTEX_POINT ( 'NONE', #9117 ) ;
#2533 = CARTESIAN_POINT ( 'NONE',  ( 0.000000000000000000, 0.000000000000000000, 0.000000000000000000 ) ) ;
#2534 = FACE_OUTER_BOUND ( 'NONE', #9884, .T. ) ;
#2535 = EDGE_LOOP ( 'NONE', ( #7510, #9842, #2068, #4600 ) ) ;
#2536 = DIRECTION ( 'NONE',  ( 0.000000000000000000, 0.000000000000000000, -1.000000000000000000 ) ) ;
#2537 = EDGE_CURVE ( 'NONE', #978, #1981, #10012, .T. ) ;
#2538 = EDGE_CURVE ( 'NONE', #9354, #5416, #4620, .T. ) ;
#2539 = ORIENTED_EDGE ( 'NONE', *, *, #883, .F. ) ;
#2540 = DIRECTION ( 'NONE',  ( -1.000000000000000000, 0.000000000000000000, 0.000000000000000000 ) ) ;
#2541 = ORIENTED_EDGE ( 'NONE', *, *, #3250, .F. ) ;
#2542 = FACE_OUTER_BOUND ( 'NONE', #6504, .T. ) ;
#2543 = ORIENTED_EDGE ( 'NONE', *, *, #2158, .F. ) ;
#2544 = CYLINDRICAL_SURFACE ( 'NONE', #9185, 9.600000000009600853 ) ;
#2545 = LINE ( 'NONE', #3558, #10976 ) ;
#2546 = ADVANCED_FACE ( 'NONE', ( #2227 ), #10729, .F. ) ;
#2547 = DIRECTION ( 'NONE',  ( -0.000000000000000000, 1.000000000000000000, -0.000000000000000000 ) ) ;
#2548 = EDGE_CURVE ( 'NONE', #4639, #4147, #10908, .T. ) ;
#2549 = CIRCLE ( 'NONE', #10753, 2.700000000000000178 ) ;
#2550 = CYLINDRICAL_SURFACE ( 'NONE', #3972, 21.00000000002100009 ) ;
#2551 = DIRECTION ( 'NONE',  ( 1.000000000000000000, -0.000000000000000000, -0.000000000000000000 ) ) ;
#2552 = ADVANCED_FACE ( 'NONE', ( #531, #2157 ), #5048, .T. ) ;
#2553 = EDGE_LOOP ( 'NONE', ( #8988, #1128, #7779, #7206, #2918, #2166, #691, #2249, #9046, #2109 ) ) ;
#2554 = ORIENTED_EDGE ( 'NONE', *, *, #1821, .T. ) ;
#2555 = CARTESIAN_POINT ( 'NONE',  ( 51.00000000000000000, 5.744562646538031281, -46.00000000000000000 ) ) ;
#2556 =( LENGTH_UNIT ( ) NAMED_UNIT ( * ) SI_UNIT ( .MILLI., .METRE. ) );
#2557 = LINE ( 'NONE', #11254, #6438 ) ;
#2558 = ORIENTED_EDGE ( 'NONE', *, *, #191, .F. ) ;
#2559 = PLANE ( 'NONE',  #1904 ) ;
#2560 = ORIENTED_EDGE ( 'NONE', *, *, #7477, .T. ) ;
#2561 = LINE ( 'NONE', #10258, #12006 ) ;
#2562 = AXIS2_PLACEMENT_3D ( 'NONE', #4360, #8189, #736 ) ;
#2563 = AXIS2_PLACEMENT_3D ( 'NONE', #2175, #7817, #7940 ) ;
#2564 = ADVANCED_BREP_SHAPE_REPRESENTATION ( '', ( #8778, #6056 ), #8843 ) ;
#2565 = DIRECTION ( 'NONE',  ( 0.000000000000000000, 0.000000000000000000, 1.000000000000000000 ) ) ;
#2566 = CARTESIAN_POINT ( 'NONE',  ( -38.00000000000000000, 7.347880794884118750E-16, 5.999999999999999112 ) ) ;
#2567 = DIRECTION ( 'NONE',  ( 0.000000000000000000, -0.000000000000000000, 1.000000000000000000 ) ) ;
#2568 = DIRECTION ( 'NONE',  ( -1.000000000000000000, 0.000000000000000000, 0.000000000000000000 ) ) ;
#2569 = AXIS2_PLACEMENT_3D ( 'NONE', #7427, #6543, #10343 ) ;
#2570 = APPLICATION_CONTEXT ( 'automotive_design' ) ;
#2571 = CIRCLE ( 'NONE', #2771, 14.24900000001425227 ) ;
#2572 = VERTEX_POINT ( 'NONE', #4107 ) ;
#2573 = CARTESIAN_POINT ( 'NONE',  ( 4.999999999999999112, 14.40062958310465469, -8.872489362018239234 ) ) ;
#2574 = DIRECTION ( 'NONE',  ( 0.000000000000000000, 0.000000000000000000, -1.000000000000000000 ) ) ;
#2575 = COLOUR_RGB ( '',1.000000000000000000, 0.9490196078431372140, 0.9098039215686274384 ) ;
#2576 = EDGE_LOOP ( 'NONE', ( #5137, #9790, #5069, #9510 ) ) ;
#2577 = CARTESIAN_POINT ( 'NONE',  ( 15.00000000000000355, 40.00000000000000711, 0.000000000000000000 ) ) ;
#2578 = ORIENTED_EDGE ( 'NONE', *, *, #10956, .T. ) ;
#2579 = VECTOR ( 'NONE', #6955, 1000.000000000000000 ) ;
#2580 = TOROIDAL_SURFACE ( 'NONE', #9389, 7.399999999999999467, 0.1000000000000000472 ) ;
#2581 = EDGE_CURVE ( 'NONE', #6339, #1692, #5417, .T. ) ;
#2582 = CARTESIAN_POINT ( 'NONE',  ( -1.500000000000001332, 8.541911424052788811E-16, 6.975000000000000533 ) ) ;
#2583 = EDGE_CURVE ( 'NONE', #3460, #12042, #1616, .T. ) ;
#2584 = VECTOR ( 'NONE', #5375, 1000.000000000000000 ) ;
#2585 = LINE ( 'NONE', #7350, #2992 ) ;
#2586 = DIRECTION ( 'NONE',  ( 0.000000000000000000, 0.000000000000000000, -1.000000000000000000 ) ) ;
#2587 = FACE_OUTER_BOUND ( 'NONE', #3038, .T. ) ;
#2588 = CARTESIAN_POINT ( 'NONE',  ( 46.00000000000000000, 1.456773409934505593E-31, -41.99999999999998579 ) ) ;
#2589 = VERTEX_POINT ( 'NONE', #2660 ) ;
#2590 = DIRECTION ( 'NONE',  ( 0.000000000000000000, 0.000000000000000000, -1.000000000000000000 ) ) ;
#2591 = VECTOR ( 'NONE', #5529, 1000.000000000000000 ) ;
#2592 = ORIENTED_EDGE ( 'NONE', *, *, #916, .F. ) ;
#2593 = DIRECTION ( 'NONE',  ( 0.000000000000000000, 0.000000000000000000, 1.000000000000000000 ) ) ;
#2594 =( LENGTH_UNIT ( ) NAMED_UNIT ( * ) SI_UNIT ( .MILLI., .METRE. ) );
#2595 = EDGE_LOOP ( 'NONE', ( #12212, #6420, #6566, #2038 ) ) ;
#2596 = AXIS2_PLACEMENT_3D ( 'NONE', #8360, #1676, #675 ) ;
#2597 = PLANE ( 'NONE',  #4213 ) ;
#2598 = FACE_OUTER_BOUND ( 'NONE', #8133, .T. ) ;
#2599 = EDGE_LOOP ( 'NONE', ( #7712, #8599, #5108 ) ) ;
#2600 = DIRECTION ( 'NONE',  ( 0.000000000000000000, 0.7071067811865439090, 0.7071067811865511255 ) ) ;
#2601 = CIRCLE ( 'NONE', #11585, 2.000000000000000000 ) ;
#2602 = CIRCLE ( 'NONE', #6209, 3.885863436426969297 ) ;
#2603 = EDGE_LOOP ( 'NONE', ( #8336, #4066 ) ) ;
#2604 = LINE ( 'NONE', #11168, #7784 ) ;
#2605 = ORIENTED_EDGE ( 'NONE', *, *, #5155, .T. ) ;
#2606 =( NAMED_UNIT ( * ) PLANE_ANGLE_UNIT ( ) SI_UNIT ( $, .RADIAN. ) );
#2607=STYLED_ITEM('',(#12384),#8751);
#2608 = FACE_BOUND ( 'NONE', #11084, .T. ) ;
#2609 = CIRCLE ( 'NONE', #11798, 0.7499999999999997780 ) ;
#2610 = ORIENTED_EDGE ( 'NONE', *, *, #4488, .T. ) ;
#2611 = CARTESIAN_POINT ( 'NONE',  ( 1.600000000000000089, 0.000000000000000000, 0.000000000000000000 ) ) ;
#2612 = AXIS2_PLACEMENT_3D ( 'NONE', #4728, #12282, #10341 ) ;
#2613 = EDGE_CURVE ( 'NONE', #10139, #12046, #8237, .T. ) ;
#2614 = CARTESIAN_POINT ( 'NONE',  ( 0.000000000000000000, 0.000000000000000000, -1.000000000000000000 ) ) ;
#2615 = MECHANICAL_DESIGN_GEOMETRIC_PRESENTATION_REPRESENTATION (  '', ( #1028 ), #9040 ) ;
#2616 = CIRCLE ( 'NONE', #24, 21.00000000002100009 ) ;
#2617 = CIRCLE ( 'NONE', #2027, 4.799999999999999822 ) ;
#2618 = AXIS2_PLACEMENT_3D ( 'NONE', #5280, #2277, #5144 ) ;
#2619 = AXIS2_PLACEMENT_3D ( 'NONE', #1145, #2858, #6491 ) ;
#2620 = DIRECTION ( 'NONE',  ( 0.000000000000000000, -0.000000000000000000, 1.000000000000000000 ) ) ;
#2621 = CARTESIAN_POINT ( 'NONE',  ( 0.000000000000000000, -0.4834863907624570856, -16.90755573046746463 ) ) ;
#2622 = ORIENTED_EDGE ( 'NONE', *, *, #6922, .T. ) ;
#2623 = VERTEX_POINT ( 'NONE', #1777 ) ;
#2624 = DIRECTION ( 'NONE',  ( 0.000000000000000000, 0.000000000000000000, 1.000000000000000000 ) ) ;
#2625 =( NAMED_UNIT ( * ) SI_UNIT ( $, .STERADIAN. ) SOLID_ANGLE_UNIT ( ) );
#2626 = DIRECTION ( 'NONE',  ( 0.000000000000000000, 0.000000000000000000, 1.000000000000000000 ) ) ;
#2627 = CARTESIAN_POINT ( 'NONE',  ( 0.000000000000000000, 0.000000000000000000, 0.000000000000000000 ) ) ;
#2628 = EDGE_CURVE ( 'NONE', #6331, #6684, #11193, .T. ) ;
#2629 = EDGE_LOOP ( 'NONE', ( #11526, #3927, #5490, #12163 ) ) ;
#2630 = LINE ( 'NONE', #8207, #11415 ) ;
#2631 =( GEOMETRIC_REPRESENTATION_CONTEXT ( 3 ) GLOBAL_UNCERTAINTY_ASSIGNED_CONTEXT ( ( #10519 ) ) GLOBAL_UNIT_ASSIGNED_CONTEXT ( ( #10862, #4054, #233 ) ) REPRESENTATION_CONTEXT ( 'NONE', 'WORKASPACE' ) );
#2632 = AXIS2_PLACEMENT_3D ( 'NONE', #2847, #6788, #11577 ) ;
#2633 = VECTOR ( 'NONE', #4313, 1000.000000000000000 ) ;
#2634 = EDGE_CURVE ( 'NONE', #2216, #6238, #10199, .T. ) ;
#2635 = AXIS2_PLACEMENT_3D ( 'NONE', #8902, #1262, #5076 ) ;
#2636 = EDGE_CURVE ( 'NONE', #11907, #8510, #10796, .T. ) ;
#2637 = CARTESIAN_POINT ( 'NONE',  ( 4.999999999999999112, -13.09267581720870766, 5.622796541391519298 ) ) ;
#2638 = CARTESIAN_POINT ( 'NONE',  ( -1.399999999999998579, 0.000000000000000000, 0.000000000000000000 ) ) ;
#2639 = ORIENTED_EDGE ( 'NONE', *, *, #12100, .T. ) ;
#2640 = DIRECTION ( 'NONE',  ( 0.000000000000000000, 0.000000000000000000, -1.000000000000000000 ) ) ;
#2641 = FACE_OUTER_BOUND ( 'NONE', #297, .T. ) ;
#2642 = AXIS2_PLACEMENT_3D ( 'NONE', #1000, #9706, #8757 ) ;
#2643 = ORIENTED_EDGE ( 'NONE', *, *, #10890, .T. ) ;
#2644 = DIRECTION ( 'NONE',  ( -1.000000000000000000, -0.000000000000000000, -0.000000000000000000 ) ) ;
#2645 = CIRCLE ( 'NONE', #853, 5.000000000000004441 ) ;
#2646 = CARTESIAN_POINT ( 'NONE',  ( 0.000000000000000000, 7.654042494670957606E-16, -6.250000000000000000 ) ) ;
#2647 = EDGE_LOOP ( 'NONE', ( #9997, #9816, #1059, #12141 ) ) ;
#2648 = LINE ( 'NONE', #11270, #475 ) ;
#2649 = ORIENTED_EDGE ( 'NONE', *, *, #2131, .F. ) ;
#2650 = EDGE_CURVE ( 'NONE', #130, #3603, #7353, .T. ) ;
#2651 = EDGE_CURVE ( 'NONE', #2486, #4605, #843, .T. ) ;
#2652 = CIRCLE ( 'NONE', #9656, 9.600000000009600853 ) ;
#2653 = EDGE_CURVE ( 'NONE', #2345, #1161, #6416, .T. ) ;
#2654 = VECTOR ( 'NONE', #3995, 1000.000000000000000 ) ;
#2655 = PLANE ( 'NONE',  #4379 ) ;
#2656 =( REPRESENTATION_RELATIONSHIP ('NONE','NONE', #9709, #1953 ) REPRESENTATION_RELATIONSHIP_WITH_TRANSFORMATION ( #7680 )SHAPE_REPRESENTATION_RELATIONSHIP( ) );
#2657 = CYLINDRICAL_SURFACE ( 'NONE', #4381, 14.24900000001425227 ) ;
#2658 = CARTESIAN_POINT ( 'NONE',  ( 4.999999999999999112, 13.09267581720874674, -5.622796541391427816 ) ) ;
#2659 = LINE ( 'NONE', #5589, #9831 ) ;
#2660 = CARTESIAN_POINT ( 'NONE',  ( 0.000000000000000000, 26.60936692326690789, -4.576198416197345686 ) ) ;
#2661 = VERTEX_POINT ( 'NONE', #1665 ) ;
#2662 = VERTEX_POINT ( 'NONE', #9300 ) ;
#2663 = CARTESIAN_POINT ( 'NONE',  ( -4.078421086530219064, -3.990950201428956845, -1.000000000000000000 ) ) ;
#2664 = VERTEX_POINT ( 'NONE', #5413 ) ;
#2665 = CARTESIAN_POINT ( 'NONE',  ( 4.999999999999999112, -1.676853263447787068, -14.14998813191271410 ) ) ;
#2666 = PRODUCT_CONTEXT ( 'NONE', #11752, 'mechanical' ) ;
#2667 = ADVANCED_FACE ( 'NONE', ( #717 ), #7302, .T. ) ;
#2668 = CIRCLE ( 'NONE', #2467, 5.100000000000000533 ) ;
#2670 = EDGE_CURVE ( 'NONE', #10975, #4084, #1623, .T. ) ;
#2669 = EDGE_LOOP ( 'NONE', ( #945, #244 ) ) ;
#2671 = DIRECTION ( 'NONE',  ( 0.000000000000000000, 0.000000000000000000, -1.000000000000000000 ) ) ;
#2672 = CARTESIAN_POINT ( 'NONE',  ( 4.999999999999999112, 13.85025647830082818, -17.79862902732250163 ) ) ;
#2673 = ORIENTED_EDGE ( 'NONE', *, *, #6635, .F. ) ;
#2674 = FACE_OUTER_BOUND ( 'NONE', #2185, .T. ) ;
#2675 = DIRECTION ( 'NONE',  ( 1.000000000000000000, 0.000000000000000000, 0.000000000000000000 ) ) ;
#2676 = ORIENTED_EDGE ( 'NONE', *, *, #2117, .T. ) ;
#2677 = DIRECTION ( 'NONE',  ( 0.000000000000000000, 0.000000000000000000, 1.000000000000000000 ) ) ;
#2678 = EDGE_LOOP ( 'NONE', ( #3346, #12181, #1566, #116 ) ) ;
#2679 = EDGE_CURVE ( 'NONE', #6067, #9683, #10623, .T. ) ;
#2680 = FACE_BOUND ( 'NONE', #10736, .T. ) ;
#2681 = CIRCLE ( 'NONE', #10077, 2.396904916527699214 ) ;
#2682 = ORIENTED_EDGE ( 'NONE', *, *, #8074, .T. ) ;
#2683 = PLANE ( 'NONE',  #7968 ) ;
#2684 = FACE_OUTER_BOUND ( 'NONE', #3723, .T. ) ;
#2685 = CIRCLE ( 'NONE', #3106, 20.24900000002024569 ) ;
#2686 = DIRECTION ( 'NONE',  ( -1.000000000000000000, -0.000000000000000000, -0.000000000000000000 ) ) ;
#2687 = CARTESIAN_POINT ( 'NONE',  ( 4.999999999999999112, 11.41582255376072830, 8.527191590521114861 ) ) ;
#2688 = ORIENTED_EDGE ( 'NONE', *, *, #7992, .T. ) ;
#2689 = ORIENTED_EDGE ( 'NONE', *, *, #3428, .F. ) ;
#2690 = CARTESIAN_POINT ( 'NONE',  ( 4.999999999999999112, 0.4834863907628118573, -16.90755573046745397 ) ) ;
#2691 = DIRECTION ( 'NONE',  ( 1.000000000000000000, 0.000000000000000000, 0.000000000000000000 ) ) ;
#2692 = DIRECTION ( 'NONE',  ( 0.000000000000000000, 0.000000000000000000, 1.000000000000000000 ) ) ;
#2693 = ORIENTED_EDGE ( 'NONE', *, *, #7950, .F. ) ;
#2694 = DIRECTION ( 'NONE',  ( 0.000000000000000000, -1.000000000000000000, 0.000000000000000000 ) ) ;
#2695 = AXIS2_PLACEMENT_3D ( 'NONE', #9940, #11549, #310 ) ;
#2696 = CARTESIAN_POINT ( 'NONE',  ( -4.799999999999999822, 5.878304635907294211E-16, -1.000000000000000000 ) ) ;
#2697 = CYLINDRICAL_SURFACE ( 'NONE', #4608, 8.099999999999999645 ) ;
#2698 = EDGE_CURVE ( 'NONE', #9964, #8188, #2427, .T. ) ;
#2699 = ORIENTED_EDGE ( 'NONE', *, *, #9732, .T. ) ;
#2700 = DIRECTION ( 'NONE',  ( 0.000000000000000000, 0.000000000000000000, 1.000000000000000000 ) ) ;
#2701 = CARTESIAN_POINT ( 'NONE',  ( -20.63749999999999574, 0.000000000000000000, 0.000000000000000000 ) ) ;
#2702 = ORIENTED_EDGE ( 'NONE', *, *, #953, .F. ) ;
#2703 = ADVANCED_FACE ( 'NONE', ( #8482 ), #4592, .T. ) ;
#2704 = CYLINDRICAL_SURFACE ( 'NONE', #10959, 5.000000000000000000 ) ;
#2705 = CARTESIAN_POINT ( 'NONE',  ( 51.00000000000000000, 3.061616997868383141E-16, -39.49999999999999289 ) ) ;
#2706 = ORIENTED_EDGE ( 'NONE', *, *, #4840, .F. ) ;
#2707 = CARTESIAN_POINT ( 'NONE',  ( 4.999999999999999112, -5.984728032765115557, 21.74405275335756116 ) ) ;
#2708 = ORIENTED_EDGE ( 'NONE', *, *, #9386, .T. ) ;
#2709 = LINE ( 'NONE', #5713, #1600 ) ;
#2710 = DIRECTION ( 'NONE',  ( -1.000000000000000000, 0.000000000000000000, 0.000000000000000000 ) ) ;
#2711 = DIRECTION ( 'NONE',  ( 1.000000000000000000, -0.000000000000000000, -0.000000000000000000 ) ) ;
#2712 = EDGE_CURVE ( 'NONE', #1460, #5665, #5224, .T. ) ;
#2713 = CARTESIAN_POINT ( 'NONE',  ( -10.00000000000000000, 0.000000000000000000, 0.000000000000000000 ) ) ;
#2714 = CARTESIAN_POINT ( 'NONE',  ( -1.400000000000001910, 0.000000000000000000, 0.000000000000000000 ) ) ;
#2715 = EDGE_LOOP ( 'NONE', ( #9455, #9983 ) ) ;
#2717 = EDGE_CURVE ( 'NONE', #4999, #6297, #1238, .T. ) ;
#2716 = ORIENTED_EDGE ( 'NONE', *, *, #2718, .T. ) ;
#2718 = EDGE_CURVE ( 'NONE', #5984, #2502, #5590, .T. ) ;
#2719 = DIRECTION ( 'NONE',  ( 2.598194829928303306E-18, 0.5446390350150290827, -0.8386705679454227180 ) ) ;
#2720 = EDGE_CURVE ( 'NONE', #12254, #2061, #3829, .T. ) ;
#2721 = ORIENTED_EDGE ( 'NONE', *, *, #1602, .F. ) ;
#2722 = DIRECTION ( 'NONE',  ( 1.000000000000000000, 0.000000000000000000, 0.000000000000000000 ) ) ;
#2723 = DIRECTION ( 'NONE',  ( 0.000000000000000000, 0.000000000000000000, 1.000000000000000000 ) ) ;
#2724 = ORIENTED_EDGE ( 'NONE', *, *, #5874, .F. ) ;
#2725 = FACE_OUTER_BOUND ( 'NONE', #2071, .T. ) ;
#2726 = CARTESIAN_POINT ( 'NONE',  ( 1.199999999999999956, 0.000000000000000000, 0.000000000000000000 ) ) ;
#2727 = ORIENTED_EDGE ( 'NONE', *, *, #5993, .F. ) ;
#2728 = ORIENTED_EDGE ( 'NONE', *, *, #2183, .T. ) ;
#2729 = CARTESIAN_POINT ( 'NONE',  ( 0.000000000000000000, -11.14352537685188338, 19.60720892790249081 ) ) ;
#2730 = DIRECTION ( 'NONE',  ( 0.000000000000000000, 0.000000000000000000, 1.000000000000000000 ) ) ;
#2731 = ORIENTED_EDGE ( 'NONE', *, *, #9079, .T. ) ;
#2732 = CARTESIAN_POINT ( 'NONE',  ( 4.999999999999999112, -11.41582255376066968, -8.527191590521194797 ) ) ;
#2733 = PRODUCT_RELATED_PRODUCT_CATEGORY ( 'part', '', ( #132 ) ) ;
#2734 = VERTEX_POINT ( 'NONE', #586 ) ;
#2735 = PLANE ( 'NONE',  #3030 ) ;
#2736 = ORIENTED_EDGE ( 'NONE', *, *, #3254, .T. ) ;
#2737 = DIRECTION ( 'NONE',  ( -0.000000000000000000, 1.000000000000000000, 0.000000000000000000 ) ) ;
#2738 = DIRECTION ( 'NONE',  ( 0.000000000000000000, 0.000000000000000000, 1.000000000000000000 ) ) ;
#2739 = EDGE_CURVE ( 'NONE', #10347, #4159, #4473, .T. ) ;
#2740 = EDGE_CURVE ( 'NONE', #7756, #7721, #9229, .T. ) ;
#2741 = CARTESIAN_POINT ( 'NONE',  ( -20.63749999999999574, 0.000000000000000000, 0.000000000000000000 ) ) ;
#2742 = DIRECTION ( 'NONE',  ( 0.000000000000000000, 0.7512545167371323940, -0.6600126143355576902 ) ) ;
#2743 = ORIENTED_EDGE ( 'NONE', *, *, #8913, .T. ) ;
#2744 = ORIENTED_EDGE ( 'NONE', *, *, #8460, .F. ) ;
#2745 = DIRECTION ( 'NONE',  ( -1.000000000000000000, -0.000000000000000000, 0.000000000000000000 ) ) ;
#2746 =( NAMED_UNIT ( * ) SI_UNIT ( $, .STERADIAN. ) SOLID_ANGLE_UNIT ( ) );
#2747 = DIRECTION ( 'NONE',  ( 0.000000000000000000, 0.000000000000000000, -1.000000000000000000 ) ) ;
#2748 = DIRECTION ( 'NONE',  ( -1.000000000000000000, -0.000000000000000000, -0.000000000000000000 ) ) ;
#2749 = ORIENTED_EDGE ( 'NONE', *, *, #10679, .F. ) ;
#2750 = PLANE ( 'NONE',  #7583 ) ;
#2751 = LINE ( 'NONE', #6576, #1613 ) ;
#2752 = CARTESIAN_POINT ( 'NONE',  ( 46.00000000000000000, 3.500000000000001332, -45.49999999999998579 ) ) ;
#2753 = ORIENTED_EDGE ( 'NONE', *, *, #6389, .T. ) ;
#2754 = CARTESIAN_POINT ( 'NONE',  ( -20.63749999999999929, 0.000000000000000000, 0.000000000000000000 ) ) ;
#2755 = CARTESIAN_POINT ( 'NONE',  ( 4.999999999999999112, -4.576198416197433616, 26.60936692326689013 ) ) ;
#2756 = ORIENTED_EDGE ( 'NONE', *, *, #1420, .F. ) ;
#2757 = DIRECTION ( 'NONE',  ( -1.000000000000000000, -0.000000000000000000, -0.000000000000000000 ) ) ;
#2758 = CARTESIAN_POINT ( 'NONE',  ( -33.00000000000000000, 0.000000000000000000, 0.000000000000000000 ) ) ;
#2759 = AXIS2_PLACEMENT_3D ( 'NONE', #11486, #3688, #1741 ) ;
#2760 = ORIENTED_EDGE ( 'NONE', *, *, #3569, .T. ) ;
#2761 = DIRECTION ( 'NONE',  ( 0.000000000000000000, 1.000000000000000000, 3.491481338843133750E-15 ) ) ;
#2762 = UNCERTAINTY_MEASURE_WITH_UNIT (LENGTH_MEASURE( 1.000000000000000082E-05 ), #8513, 'distance_accuracy_value', 'NONE');
#2763 = AXIS2_PLACEMENT_3D ( 'NONE', #2741, #3883, #11490 ) ;
#2764 = EDGE_LOOP ( 'NONE', ( #1329, #2839 ) ) ;
#2765 = AXIS2_PLACEMENT_3D ( 'NONE', #10092, #7286, #4572 ) ;
#2766 = EDGE_CURVE ( 'NONE', #4747, #9384, #958, .T. ) ;
#2767 = PRESENTATION_STYLE_ASSIGNMENT (( #3772 ) ) ;
#2768 = AXIS2_PLACEMENT_3D ( 'NONE', #10060, #9070, #2415 ) ;
#2769 = CARTESIAN_POINT ( 'NONE',  ( 5.000000000000000000, 6.799999999999999822, 0.000000000000000000 ) ) ;
#2770 = CARTESIAN_POINT ( 'NONE',  ( 4.999999999999999112, 14.41081992069309869, 22.83261415639507774 ) ) ;
#2771 = AXIS2_PLACEMENT_3D ( 'NONE', #541, #9317, #9188 ) ;
#2772 = CARTESIAN_POINT ( 'NONE',  ( 0.000000000000000000, -13.09267581720870766, 5.622796541391519298 ) ) ;
#2773 = CARTESIAN_POINT ( 'NONE',  ( 46.00000000000000000, -3.499999999999998668, -38.49999999999998579 ) ) ;
#2774 = EDGE_LOOP ( 'NONE', ( #2610, #2967, #2852, #9776 ) ) ;
#2775 = ORIENTED_EDGE ( 'NONE', *, *, #4149, .T. ) ;
#2776 = DIRECTION ( 'NONE',  ( 0.000000000000000000, 0.000000000000000000, 1.000000000000000000 ) ) ;
#2777 = ORIENTED_EDGE ( 'NONE', *, *, #8695, .F. ) ;
#2778 = DIRECTION ( 'NONE',  ( 1.000000000000000000, 0.000000000000000000, 0.000000000000000000 ) ) ;
#2779 = VERTEX_POINT ( 'NONE', #3963 ) ;
#2781 = DIRECTION ( 'NONE',  ( 0.000000000000000000, 0.000000000000000000, 1.000000000000000000 ) ) ;
#2780 = AXIS2_PLACEMENT_3D ( 'NONE', #6742, #9613, #8734 ) ;
#2782 = AXIS2_PLACEMENT_3D ( 'NONE', #3503, #612, #12052 ) ;
#2783 = ADVANCED_FACE ( 'NONE', ( #906, #23 ), #4906, .F. ) ;
#2784 = FACE_OUTER_BOUND ( 'NONE', #5487, .T. ) ;
#2785 = CIRCLE ( 'NONE', #6373, 27.00000000002699707 ) ;
#2786 = EDGE_CURVE ( 'NONE', #7042, #11053, #9836, .T. ) ;
#2787 = ORIENTED_EDGE ( 'NONE', *, *, #809, .F. ) ;
#2788 = ADVANCED_FACE ( 'NONE', ( #4960 ), #11330, .T. ) ;
#2789 = ORIENTED_EDGE ( 'NONE', *, *, #883, .T. ) ;
#2790 = DIRECTION ( 'NONE',  ( 0.000000000000000000, 0.000000000000000000, 1.000000000000000000 ) ) ;
#2791 = DIRECTION ( 'NONE',  ( -1.000000000000000000, -0.000000000000000000, -0.000000000000000000 ) ) ;
#2792 = CYLINDRICAL_SURFACE ( 'NONE', #4407, 20.24900000002024569 ) ;
#2793 = CIRCLE ( 'NONE', #6393, 7.500000000000000000 ) ;
#2794 = VERTEX_POINT ( 'NONE', #3849 ) ;
#2795 = DIRECTION ( 'NONE',  ( 0.000000000000000000, 0.000000000000000000, 1.000000000000000000 ) ) ;
#2796 = VERTEX_POINT ( 'NONE', #3034 ) ;
#2797 = SHAPE_REPRESENTATION_RELATIONSHIP ( 'NONE' , 'NONE' ,  #1953, #4814 ) ;
#2798 = ORIENTED_EDGE ( 'NONE', *, *, #3294, .F. ) ;
#2799 = CARTESIAN_POINT ( 'NONE',  ( -0.5000000000000000000, -6.429618962271402616, -1.000000000000000000 ) ) ;
#2800 = VERTEX_POINT ( 'NONE', #10526 ) ;
#2801 = DIRECTION ( 'NONE',  ( 0.000000000000000000, 0.000000000000000000, -1.000000000000000000 ) ) ;
#2802 = AXIS2_PLACEMENT_3D ( 'NONE', #5540, #7608, #10290 ) ;
#2803 = EDGE_CURVE ( 'NONE', #1424, #1709, #5830, .T. ) ;
#2804 = CARTESIAN_POINT ( 'NONE',  ( -4.078421086530219064, -3.990950201428956845, 0.000000000000000000 ) ) ;
#2805 = CYLINDRICAL_SURFACE ( 'NONE', #2763, 6.750000000000000000 ) ;
#2806 = DIRECTION ( 'NONE',  ( 0.000000000000000000, 0.000000000000000000, 1.000000000000000000 ) ) ;
#2807 = AXIS2_PLACEMENT_3D ( 'NONE', #6714, #1078, #10568 ) ;
#2808 = ORIENTED_EDGE ( 'NONE', *, *, #547, .T. ) ;
#2809 = ORIENTED_EDGE ( 'NONE', *, *, #3047, .T. ) ;
#2810 = DIRECTION ( 'NONE',  ( 1.000000000000000000, 3.903127820947815962E-18, 0.000000000000000000 ) ) ;
#2811 =( NAMED_UNIT ( * ) SI_UNIT ( $, .STERADIAN. ) SOLID_ANGLE_UNIT ( ) );
#2812 = AXIS2_PLACEMENT_3D ( 'NONE', #2439, #6193, #618 ) ;
#2813 = CARTESIAN_POINT ( 'NONE',  ( 37.00000000000000711, -2.172883482918394282, 4.280020720704565740 ) ) ;
#2814 = AXIS2_PLACEMENT_3D ( 'NONE', #1794, #5495, #2600 ) ;
#2815 = DIRECTION ( 'NONE',  ( -1.000000000000000000, -0.000000000000000000, -0.000000000000000000 ) ) ;
#2816 = EDGE_CURVE ( 'NONE', #5214, #10090, #7674, .T. ) ;
#2817 = ORIENTED_EDGE ( 'NONE', *, *, #74, .F. ) ;
#2818 = DIRECTION ( 'NONE',  ( 1.000000000000000000, 0.000000000000000000, 0.000000000000000000 ) ) ;
#2819 = EDGE_CURVE ( 'NONE', #11589, #4096, #7431, .T. ) ;
#2820 = APPLICATION_CONTEXT ( 'automotive_design' ) ;
#2821 = AXIS2_PLACEMENT_3D ( 'NONE', #4721, #664, #7600 ) ;
#2822 = VECTOR ( 'NONE', #6496, 1000.000000000000000 ) ;
#2823 = CIRCLE ( 'NONE', #1224, 5.000000000000000000 ) ;
#2824 = AXIS2_PLACEMENT_3D ( 'NONE', #1555, #5376, #1050 ) ;
#2825 = VECTOR ( 'NONE', #2480, 1000.000000000000114 ) ;
#2826 = PRESENTATION_STYLE_ASSIGNMENT (( #9464 ) ) ;
#2827 = CARTESIAN_POINT ( 'NONE',  ( -1.500000000000001332, 0.000000000000000000, 0.000000000000000000 ) ) ;
#2828 = DIRECTION ( 'NONE',  ( 1.000000000000000000, 0.000000000000000000, 0.000000000000000000 ) ) ;
#2829 = CARTESIAN_POINT ( 'NONE',  ( 4.999999999999999112, 22.37914155802285876, 6.808078995945277434 ) ) ;
#2830 = EDGE_LOOP ( 'NONE', ( #3983, #4790 ) ) ;
#2831 = DIRECTION ( 'NONE',  ( 0.000000000000000000, 0.000000000000000000, -1.000000000000000000 ) ) ;
#2832 = CYLINDRICAL_SURFACE ( 'NONE', #8626, 4.799999999999999822 ) ;
#2833 = MECHANICAL_DESIGN_GEOMETRIC_PRESENTATION_REPRESENTATION (  '', ( #8831 ), #21 ) ;
#2834 = AXIS2_PLACEMENT_3D ( 'NONE', #1776, #9482, #5412 ) ;
#2835 = ORIENTED_EDGE ( 'NONE', *, *, #7796, .F. ) ;
#2836 = DIRECTION ( 'NONE',  ( 0.000000000000000000, 0.000000000000000000, -1.000000000000000000 ) ) ;
#2837 = AXIS2_PLACEMENT_3D ( 'NONE', #1126, #10446, #4937 ) ;
#2838 = VECTOR ( 'NONE', #10774, 1000.000000000000000 ) ;
#2839 = ORIENTED_EDGE ( 'NONE', *, *, #4092, .T. ) ;
#2840 = AXIS2_PLACEMENT_3D ( 'NONE', #3637, #11258, #6515 ) ;
#2841 = FACE_OUTER_BOUND ( 'NONE', #4910, .T. ) ;
#2842 = AXIS2_PLACEMENT_3D ( 'NONE', #11937, #3392, #2389 ) ;
#2843 = CIRCLE ( 'NONE', #6851, 2.055000000000000160 ) ;
#2844 = CARTESIAN_POINT ( 'NONE',  ( -33.00000000000000000, 0.000000000000000000, 6.500000000000000888 ) ) ;
#2845 = FACE_OUTER_BOUND ( 'NONE', #1678, .T. ) ;
#2846 = AXIS2_PLACEMENT_3D ( 'NONE', #10387, #4650, #12311 ) ;
#2847 = CARTESIAN_POINT ( 'NONE',  ( 0.000000000000000000, 19.60720892790252989, -11.14352537685181588 ) ) ;
#2848 = CARTESIAN_POINT ( 'NONE',  ( 16.55500000000001393, 3.061616997868383634E-16, -2.500000000000000444 ) ) ;
#2849 = EDGE_LOOP ( 'NONE', ( #6528, #7916, #3456, #10520 ) ) ;
#2850 = ORIENTED_EDGE ( 'NONE', *, *, #5097, .F. ) ;
#2851 = CYLINDRICAL_SURFACE ( 'NONE', #257, 6.500000000000000888 ) ;
#2852 = ORIENTED_EDGE ( 'NONE', *, *, #10196, .T. ) ;
#2853 = DIRECTION ( 'NONE',  ( 1.000000000000000000, 0.000000000000000000, 0.000000000000000000 ) ) ;
#2854 = PRODUCT_CONTEXT ( 'NONE', #4738, 'mechanical' ) ;
#2855 = ORIENTED_EDGE ( 'NONE', *, *, #296, .F. ) ;
#2856 = EDGE_LOOP ( 'NONE', ( #3042, #4731, #346, #8495 ) ) ;
#2857 = AXIS2_PLACEMENT_3D ( 'NONE', #9654, #9468, #1081 ) ;
#2858 = DIRECTION ( 'NONE',  ( 1.000000000000000000, 0.000000000000000000, 0.000000000000000000 ) ) ;
#2859 = AXIS2_PLACEMENT_3D ( 'NONE', #6449, #10250, #740 ) ;
#2860 = CARTESIAN_POINT ( 'NONE',  ( -20.00000000000000000, 40.00000000000000711, -12.50000000000000000 ) ) ;
#2861 = ORIENTED_EDGE ( 'NONE', *, *, #7930, .T. ) ;
#2862 = EDGE_LOOP ( 'NONE', ( #2554, #9744, #4768, #5323 ) ) ;
#2863 = CARTESIAN_POINT ( 'NONE',  ( 2.500000000000000000, 2.357898499370433054, -1.951563910473907981E-15 ) ) ;
#2864 = DIRECTION ( 'NONE',  ( -1.000000000000000000, -0.000000000000000000, -0.000000000000000000 ) ) ;
#2865 = CARTESIAN_POINT ( 'NONE',  ( 0.4795650472149387000, 0.5999999999999996447, 3.611001245881807264 ) ) ;
#2866 = LINE ( 'NONE', #3979, #11990 ) ;
#2867 = EDGE_CURVE ( 'NONE', #4122, #214, #3911, .T. ) ;
#2868 = ORIENTED_EDGE ( 'NONE', *, *, #9322, .F. ) ;
#2869 = AXIS2_PLACEMENT_3D ( 'NONE', #7941, #4121, #9754 ) ;
#2870 = DIRECTION ( 'NONE',  ( -1.000000000000000000, -0.000000000000000000, -0.000000000000000000 ) ) ;
#2871 = ORIENTED_EDGE ( 'NONE', *, *, #10670, .T. ) ;
#2872 = ADVANCED_FACE ( 'NONE', ( #7729 ), #5855, .T. ) ;
#2873 =( NAMED_UNIT ( * ) PLANE_ANGLE_UNIT ( ) SI_UNIT ( $, .RADIAN. ) );
#2874 = EDGE_LOOP ( 'NONE', ( #11142, #7666, #363, #7895 ) ) ;
#2875 = CARTESIAN_POINT ( 'NONE',  ( 1.500000000000000888, 6.245698675651501825E-16, 5.100000000000000533 ) ) ;
#2876 = ORIENTED_EDGE ( 'NONE', *, *, #7490, .F. ) ;
#2877 = CARTESIAN_POINT ( 'NONE',  ( 15.00000000000000355, 40.00000000000000711, 1.999999999999998224 ) ) ;
#2878 = CARTESIAN_POINT ( 'NONE',  ( 1.500000000000001332, 9.123618653647779187E-16, 7.399999999999999467 ) ) ;
#2879 = EDGE_CURVE ( 'NONE', #1723, #2076, #10212, .T. ) ;
#2880 = CARTESIAN_POINT ( 'NONE',  ( -20.63749999999999574, 0.000000000000000000, -6.975000000000000533 ) ) ;
#2881 = LINE ( 'NONE', #7568, #3459 ) ;
#2882 = ORIENTED_EDGE ( 'NONE', *, *, #4483, .T. ) ;
#2883 = CARTESIAN_POINT ( 'NONE',  ( 4.999999999999999112, -20.18872947935930284, -1.561154383803435408 ) ) ;
#2884 = EDGE_CURVE ( 'NONE', #10051, #7451, #8597, .T. ) ;
#2885 = VECTOR ( 'NONE', #9967, 1000.000000000000000 ) ;
#2886 = SURFACE_SIDE_STYLE ('',( #999 ) ) ;
#2887 = FACE_OUTER_BOUND ( 'NONE', #5644, .T. ) ;
#2888 = EDGE_CURVE ( 'NONE', #2328, #6849, #5624, .T. ) ;
#2889 = EDGE_CURVE ( 'NONE', #8025, #11929, #1433, .T. ) ;
#2890 = DIRECTION ( 'NONE',  ( 0.000000000000000000, 0.000000000000000000, -1.000000000000000000 ) ) ;
#2891 = ORIENTED_EDGE ( 'NONE', *, *, #3710, .T. ) ;
#2892 = DIRECTION ( 'NONE',  ( 1.000000000000000000, 0.000000000000000000, 0.000000000000000000 ) ) ;
#2893 = VECTOR ( 'NONE', #1268, 1000.000000000000000 ) ;
#2894 = CARTESIAN_POINT ( 'NONE',  ( -10.00000000000000000, 0.000000000000000000, 0.000000000000000000 ) ) ;
#2895 = DIRECTION ( 'NONE',  ( -1.000000000000000000, 0.000000000000000000, -0.000000000000000000 ) ) ;
#2896 = EDGE_CURVE ( 'NONE', #1494, #9332, #8834, .T. ) ;
#2897 = DIRECTION ( 'NONE',  ( 0.000000000000000000, 0.000000000000000000, 1.000000000000000000 ) ) ;
#2898 = LINE ( 'NONE', #2950, #7041 ) ;
#2899 = EDGE_LOOP ( 'NONE', ( #10933, #2313, #4925, #5764 ) ) ;
#2900 = DIRECTION ( 'NONE',  ( 0.000000000000000000, 0.000000000000000000, 1.000000000000000000 ) ) ;
#2901 = DIRECTION ( 'NONE',  ( 0.000000000000000000, 0.6828850436591804574, 0.7305258497456468270 ) ) ;
#2902 = ORIENTED_EDGE ( 'NONE', *, *, #11124, .T. ) ;
#2903 = CARTESIAN_POINT ( 'NONE',  ( 2.499999999999999556, -20.41639017900856246, -4.916402349214798129 ) ) ;
#2904 = AXIS2_PLACEMENT_3D ( 'NONE', #7004, #6070, #6004 ) ;
#2905 = ORIENTED_EDGE ( 'NONE', *, *, #7613, .F. ) ;
#2906 = DIRECTION ( 'NONE',  ( 0.000000000000000000, -1.000000000000000000, 0.000000000000000000 ) ) ;
#2907 = CYLINDRICAL_SURFACE ( 'NONE', #12173, 0.7500000000000000000 ) ;
#2908 = DIRECTION ( 'NONE',  ( -1.000000000000000000, 0.000000000000000000, 0.000000000000000000 ) ) ;
#2909 = AXIS2_PLACEMENT_3D ( 'NONE', #10068, #7264, #4357 ) ;
#2910 = EDGE_CURVE ( 'NONE', #9806, #7902, #619, .T. ) ;
#2911 = LINE ( 'NONE', #4775, #10033 ) ;
#2912 = DIRECTION ( 'NONE',  ( 0.000000000000000000, 0.000000000000000000, 1.000000000000000000 ) ) ;
#2913 = VERTEX_POINT ( 'NONE', #11397 ) ;
#2914 = EDGE_LOOP ( 'NONE', ( #7933, #4511, #5973, #1682, #1410, #12158, #11727, #539, #8955, #3912, #4287, #6695, #5729, #6234, #10391, #6437, #8922, #1033, #4967, #731 ) ) ;
#2915 = LINE ( 'NONE', #9730, #10436 ) ;
#2916 = ORIENTED_EDGE ( 'NONE', *, *, #11833, .F. ) ;
#2917 = DIRECTION ( 'NONE',  ( -1.000000000000000000, -0.000000000000000000, -0.000000000000000000 ) ) ;
#2918 = ORIENTED_EDGE ( 'NONE', *, *, #2432, .T. ) ;
#2919 = ORIENTED_EDGE ( 'NONE', *, *, #6845, .T. ) ;
#2920 = ORIENTED_EDGE ( 'NONE', *, *, #2889, .T. ) ;
#2921 = CYLINDRICAL_SURFACE ( 'NONE', #2780, 27.00000000002699707 ) ;
#2922 = CARTESIAN_POINT ( 'NONE',  ( 1.250000000000000000, -6.429618962271402616, -1.000000000000000000 ) ) ;
#2923 = CARTESIAN_POINT ( 'NONE',  ( 33.00000000000000000, 0.000000000000000000, -41.99999999999999289 ) ) ;
#2924 = DIRECTION ( 'NONE',  ( 0.000000000000000000, 0.000000000000000000, -1.000000000000000000 ) ) ;
#2925 = ORIENTED_EDGE ( 'NONE', *, *, #10981, .F. ) ;
#2926 = DIRECTION ( 'NONE',  ( 0.000000000000000000, 0.7900737791495477946, 0.6130117645692876316 ) ) ;
#2927 = VERTEX_POINT ( 'NONE', #2848 ) ;
#2928 = SURFACE_STYLE_USAGE ( .BOTH. , #1738 ) ;
#2929 = ORIENTED_EDGE ( 'NONE', *, *, #785, .F. ) ;
#2930 = DIRECTION ( 'NONE',  ( 2.817067928751547788E-17, 0.6371047110838219396, -0.7707772616747329275 ) ) ;
#2931 = ORIENTED_EDGE ( 'NONE', *, *, #5478, .T. ) ;
#2932 = DIRECTION ( 'NONE',  ( -2.598194829928303306E-18, -0.5446390350150290827, 0.8386705679454227180 ) ) ;
#2933 = EDGE_CURVE ( 'NONE', #1899, #5455, #9630, .T. ) ;
#2934 = FACE_OUTER_BOUND ( 'NONE', #7625, .T. ) ;
#2935 = ADVANCED_FACE ( 'NONE', ( #278 ), #9789, .F. ) ;
#2936 = FACE_BOUND ( 'NONE', #912, .T. ) ;
#2937 = CARTESIAN_POINT ( 'NONE',  ( 1.000000000000000000, 0.000000000000000000, 0.000000000000000000 ) ) ;
#2938 = ORIENTED_EDGE ( 'NONE', *, *, #4223, .T. ) ;
#2939 = CARTESIAN_POINT ( 'NONE',  ( 26.00000000000000355, 0.000000000000000000, 0.000000000000000000 ) ) ;
#2940 = CYLINDRICAL_SURFACE ( 'NONE', #4041, 9.600000000009599077 ) ;
#2941 = CYLINDRICAL_SURFACE ( 'NONE', #6493, 6.500000000000000888 ) ;
#2942 = VERTEX_POINT ( 'NONE', #8968 ) ;
#2943 = DIRECTION ( 'NONE',  ( 0.000000000000000000, 9.486769009248163798E-17, -1.000000000000000000 ) ) ;
#2944 = EDGE_CURVE ( 'NONE', #1270, #4573, #7150, .T. ) ;
#2945 = EDGE_CURVE ( 'NONE', #7805, #12088, #11413, .T. ) ;
#2946 = EDGE_CURVE ( 'NONE', #4193, #6538, #10897, .T. ) ;
#2947 =( NAMED_UNIT ( * ) SI_UNIT ( $, .STERADIAN. ) SOLID_ANGLE_UNIT ( ) );
#2948 = DIRECTION ( 'NONE',  ( 0.000000000000000000, 0.000000000000000000, 1.000000000000000000 ) ) ;
#2949 = CARTESIAN_POINT ( 'NONE',  ( 1.250000000000000000, -6.429618962271402616, -1.000000000000000000 ) ) ;
#2950 = CARTESIAN_POINT ( 'NONE',  ( 0.000000000000000000, 0.000000000000000000, -3.790027207537782772 ) ) ;
#2951 = ORIENTED_EDGE ( 'NONE', *, *, #2128, .F. ) ;
#2952 = DIRECTION ( 'NONE',  ( -1.000000000000000000, 0.000000000000000000, 0.000000000000000000 ) ) ;
#2953 = CARTESIAN_POINT ( 'NONE',  ( 0.000000000000000000, 0.000000000000000000, -1.000000000000000000 ) ) ;
#2954 = ORIENTED_EDGE ( 'NONE', *, *, #2402, .T. ) ;
#2955 = DIRECTION ( 'NONE',  ( 0.000000000000000000, 0.000000000000000000, 1.000000000000000000 ) ) ;
#2956 = ORIENTED_EDGE ( 'NONE', *, *, #7064, .F. ) ;
#2957 = SURFACE_STYLE_FILL_AREA ( #4714 ) ;
#2958 = EDGE_CURVE ( 'NONE', #5581, #10639, #4203, .T. ) ;
#2959 = DIRECTION ( 'NONE',  ( 0.000000000000000000, -6.987080667121815555E-15, 1.000000000000000000 ) ) ;
#2960 = FACE_OUTER_BOUND ( 'NONE', #5300, .T. ) ;
#2961 = CARTESIAN_POINT ( 'NONE',  ( 0.000000000000000000, 0.000000000000000000, -1.500000000000000000 ) ) ;
#2962 = DIRECTION ( 'NONE',  ( 0.000000000000000000, 0.000000000000000000, 1.000000000000000000 ) ) ;
#2963 = ORIENTED_EDGE ( 'NONE', *, *, #9698, .T. ) ;
#2964 = ORIENTED_EDGE ( 'NONE', *, *, #2433, .F. ) ;
#2965 = FACE_OUTER_BOUND ( 'NONE', #10403, .T. ) ;
#2966 = AXIS2_PLACEMENT_3D ( 'NONE', #12321, #10399, #11576 ) ;
#2967 = ORIENTED_EDGE ( 'NONE', *, *, #7974, .T. ) ;
#2968 = PLANE ( 'NONE',  #877 ) ;
#2969 = ITEM_DEFINED_TRANSFORMATION ( 'NONE', 'NONE', #12021,  #6056 ) ;
#2970 = ORIENTED_EDGE ( 'NONE', *, *, #3515, .F. ) ;
#2971 = EDGE_CURVE ( 'NONE', #5514, #7042, #2224, .T. ) ;
#2972 = EDGE_CURVE ( 'NONE', #7442, #3694, #11801, .T. ) ;
#2973 = VECTOR ( 'NONE', #6683, 1000.000000000000000 ) ;
#2974 = AXIS2_PLACEMENT_3D ( 'NONE', #11545, #2997, #11363 ) ;
#2975 = EDGE_LOOP ( 'NONE', ( #10371, #11187, #11090, #98 ) ) ;
#2976 = EDGE_LOOP ( 'NONE', ( #2335, #11911, #8598, #7319 ) ) ;
#2977 = CARTESIAN_POINT ( 'NONE',  ( 1.000000000000000000, 0.5999999999999998668, -3.826895796574397046 ) ) ;
#2978 = CARTESIAN_POINT ( 'NONE',  ( 1.000000000000000000, 0.5999999999999998668, 4.000000000000000000 ) ) ;
#2979 = CARTESIAN_POINT ( 'NONE',  ( 37.00000000000000711, 1.456773409934505593E-31, -41.99999999999998579 ) ) ;
#2980 = CARTESIAN_POINT ( 'NONE',  ( 45.00000000000000000, 0.000000000000000000, 5.000000000000000000 ) ) ;
#2981 = ORIENTED_EDGE ( 'NONE', *, *, #2031, .F. ) ;
#2982 = DIRECTION ( 'NONE',  ( -1.000000000000000000, -0.000000000000000000, 0.000000000000000000 ) ) ;
#2983 = AXIS2_PLACEMENT_3D ( 'NONE', #9772, #2196, #139 ) ;
#2984 = ORIENTED_EDGE ( 'NONE', *, *, #4535, .T. ) ;
#2985 = VECTOR ( 'NONE', #12159, 1000.000000000000000 ) ;
#2986 =( NAMED_UNIT ( * ) PLANE_ANGLE_UNIT ( ) SI_UNIT ( $, .RADIAN. ) );
#2987 = VERTEX_POINT ( 'NONE', #2210 ) ;
#2988 = CLOSED_SHELL ( 'NONE', ( #5813, #5217, #3491, #8176, #5004, #4607, #4938, #11804, #6014, #11882, #2179, #7611 ) ) ;
#2989 = DIRECTION ( 'NONE',  ( 0.000000000000000000, 0.000000000000000000, -1.000000000000000000 ) ) ;
#2990 = VERTEX_POINT ( 'NONE', #329 ) ;
#2991 = LINE ( 'NONE', #8810, #10752 ) ;
#2992 = VECTOR ( 'NONE', #6410, 1000.000000000000000 ) ;
#2993 = VECTOR ( 'NONE', #9648, 1000.000000000000000 ) ;
#2994 = LINE ( 'NONE', #10496, #5001 ) ;
#2995 = CIRCLE ( 'NONE', #387, 7.500000000000000000 ) ;
#2996 = VERTEX_POINT ( 'NONE', #10847 ) ;
#2997 = DIRECTION ( 'NONE',  ( -1.000000000000000000, -0.000000000000000000, -0.000000000000000000 ) ) ;
#2998 = DIRECTION ( 'NONE',  ( 1.000000000000000000, 0.000000000000000000, 0.000000000000000000 ) ) ;
#2999 = EDGE_LOOP ( 'NONE', ( #8771, #2488, #11058, #5707 ) ) ;
#3000 = FACE_OUTER_BOUND ( 'NONE', #8809, .T. ) ;
#3001 =( LENGTH_UNIT ( ) NAMED_UNIT ( * ) SI_UNIT ( .MILLI., .METRE. ) );
#3002 = FACE_OUTER_BOUND ( 'NONE', #7243, .T. ) ;
#3003 = CIRCLE ( 'NONE', #395, 0.7500000000000000000 ) ;
#3004 = CARTESIAN_POINT ( 'NONE',  ( -10.00000000000000000, 0.000000000000000000, 0.000000000000000000 ) ) ;
#3005 = EDGE_CURVE ( 'NONE', #11926, #11497, #1034, .T. ) ;
#3006 = ORIENTED_EDGE ( 'NONE', *, *, #3674, .F. ) ;
#3007 = DIRECTION ( 'NONE',  ( -0.000000000000000000, 1.000000000000000000, -0.000000000000000000 ) ) ;
#3008 = CIRCLE ( 'NONE', #7008, 5.000000000000000000 ) ;
#3009=STYLED_ITEM('',(#12405),#8531);
#3010 = DIRECTION ( 'NONE',  ( 0.000000000000000000, -0.4999999999999888978, -0.8660254037844450359 ) ) ;
#3011 = CARTESIAN_POINT ( 'NONE',  ( 0.000000000000000000, 0.000000000000000000, 0.000000000000000000 ) ) ;
#3012 = AXIS2_PLACEMENT_3D ( 'NONE', #4006, #11690, #314 ) ;
#3013 = AXIS2_PLACEMENT_3D ( 'NONE', #8253, #5546, #6432 ) ;
#3014 = CARTESIAN_POINT ( 'NONE',  ( -26.00000000000000355, 30.00000000000000711, 20.00000000000001066 ) ) ;
#3015 = DIRECTION ( 'NONE',  ( 0.000000000000000000, 0.000000000000000000, -1.000000000000000000 ) ) ;
#3016 = ORIENTED_EDGE ( 'NONE', *, *, #3877, .T. ) ;
#3017 = EDGE_CURVE ( 'NONE', #8676, #6734, #3104, .T. ) ;
#3018 = CARTESIAN_POINT ( 'NONE',  ( 4.999999999999999112, 8.872489362018189496, 14.40062958310468666 ) ) ;
#3019 = DIRECTION ( 'NONE',  ( -0.000000000000000000, 1.000000000000000000, -0.000000000000000000 ) ) ;
#3020 = EDGE_LOOP ( 'NONE', ( #3175, #3631, #12291, #5387, #9567, #11463, #3509, #3744, #10426, #11532, #8712, #1056, #10101, #2507, #5882, #1426, #8110, #11225, #11995, #2931, #11909, #3108, #2809, #8828, #12335, #4566, #5162, #4206, #2956, #7908, #3917, #11874, #10952, #3919, #4515, #5928, #11365, #2174, #8575, #450, #1178, #7054, #7931, #3988, #11877, #223, #34, #7861, #5977, #9792, #9004, #2448, #407 ) ) ;
#3021 = LINE ( 'NONE', #950, #10272 ) ;
#3022 = PRODUCT_DEFINITION_CONTEXT ( 'detailed design', #10723, 'design' ) ;
#3023 = EDGE_CURVE ( 'NONE', #972, #7961, #2326, .T. ) ;
#3024 = ORIENTED_EDGE ( 'NONE', *, *, #4423, .F. ) ;
#3025 = ADVANCED_FACE ( 'NONE', ( #6037 ), #461, .T. ) ;
#3026 = COLOUR_RGB ( '',1.000000000000000000, 0.9490196078431372140, 0.9098039215686274384 ) ;
#3027 = VECTOR ( 'NONE', #10207, 1000.000000000000000 ) ;
#3028 = AXIS2_PLACEMENT_3D ( 'NONE', #11775, #8985, #10050 ) ;
#3029 = AXIS2_PLACEMENT_3D ( 'NONE', #1590, #2586, #11956 ) ;
#3030 = AXIS2_PLACEMENT_3D ( 'NONE', #6554, #10360, #1802 ) ;
#3031 = DIRECTION ( 'NONE',  ( 1.000000000000000000, -0.000000000000000000, -0.000000000000000000 ) ) ;
#3032 = CARTESIAN_POINT ( 'NONE',  ( 0.000000000000000000, 6.799999999999999822, 0.000000000000000000 ) ) ;
#3033 = CARTESIAN_POINT ( 'NONE',  ( 4.999999999999999112, 2.791921004064247480, 22.37914155802286942 ) ) ;
#3034 = CARTESIAN_POINT ( 'NONE',  ( 0.000000000000000000, -4.916402349214727963, 20.41639017900857667 ) ) ;
#3035 = CIRCLE ( 'NONE', #7224, 2.700000000000000622 ) ;
#3036 = VECTOR ( 'NONE', #3454, 1000.000000000000000 ) ;
#3037 = PRODUCT ( 'angular contact ball bearing_68_iso_ISO 15 ABB - 1710 - 20,SI,NC,20_68', 'angular contact ball bearing_68_iso_ISO 15 ABB - 1710 - 20,SI,NC,20_68', '', ( #12216 ) ) ;
#3038 = EDGE_LOOP ( 'NONE', ( #9678, #1829, #152, #55 ) ) ;
#3039 = AXIS2_PLACEMENT_3D ( 'NONE', #8416, #3665, #2472 ) ;
#3040 = CARTESIAN_POINT ( 'NONE',  ( 0.000000000000000000, 0.000000000000000000, -1.000000000000000000 ) ) ;
#3041 = VECTOR ( 'NONE', #2510, 1000.000000000000000 ) ;
#3042 = ORIENTED_EDGE ( 'NONE', *, *, #822, .T. ) ;
#3043 = EDGE_CURVE ( 'NONE', #8435, #8560, #9036, .T. ) ;
#3044 = CONTEXT_DEPENDENT_SHAPE_REPRESENTATION ( #5373, #9833 ) ;
#3045 = EDGE_CURVE ( 'NONE', #9490, #681, #4090, .T. ) ;
#3046 = ORIENTED_EDGE ( 'NONE', *, *, #6922, .F. ) ;
#3047 = EDGE_CURVE ( 'NONE', #4839, #8928, #8849, .T. ) ;
#3048 =( GEOMETRIC_REPRESENTATION_CONTEXT ( 3 ) GLOBAL_UNCERTAINTY_ASSIGNED_CONTEXT ( ( #8161 ) ) GLOBAL_UNIT_ASSIGNED_CONTEXT ( ( #425, #2873, #9440 ) ) REPRESENTATION_CONTEXT ( 'NONE', 'WORKASPACE' ) );
#3049 = CIRCLE ( 'NONE', #4426, 5.525000000000000355 ) ;
#3050 = AXIS2_PLACEMENT_3D ( 'NONE', #3833, #10458, #11448 ) ;
#3051 = DIRECTION ( 'NONE',  ( -0.000000000000000000, 1.000000000000000000, 1.224646799147353207E-16 ) ) ;
#3052 = ORIENTED_EDGE ( 'NONE', *, *, #11051, .T. ) ;
#3053 = LINE ( 'NONE', #8610, #4796 ) ;
#3054 = FACE_OUTER_BOUND ( 'NONE', #847, .T. ) ;
#3055 = DIRECTION ( 'NONE',  ( -1.000000000000000000, -0.000000000000000000, 0.000000000000000000 ) ) ;
#3056 = LINE ( 'NONE', #11666, #5020 ) ;
#3057 = VERTEX_POINT ( 'NONE', #10948 ) ;
#3058 = EDGE_CURVE ( 'NONE', #6875, #7704, #11703, .T. ) ;
#3059 = ADVANCED_FACE ( 'NONE', ( #9861 ), #11652, .T. ) ;
#3061 = CARTESIAN_POINT ( 'NONE',  ( 2.500000000000000000, 2.357898499370433054, -1.951563910473907981E-15 ) ) ;
#3060 = MECHANICAL_DESIGN_GEOMETRIC_PRESENTATION_REPRESENTATION (  '', ( #7045 ), #5050 ) ;
#3062 = AXIS2_PLACEMENT_3D ( 'NONE', #11201, #7341, #2567 ) ;
#3063 = ORIENTED_EDGE ( 'NONE', *, *, #10799, .T. ) ;
#3064 = VECTOR ( 'NONE', #6298, 1000.000000000000000 ) ;
#3065 = PRODUCT_CONTEXT ( 'NONE', #3872, 'mechanical' ) ;
#3066 = AXIS2_PLACEMENT_3D ( 'NONE', #9453, #8450, #10369 ) ;
#3067 = ORIENTED_EDGE ( 'NONE', *, *, #9209, .T. ) ;
#3068 = FACE_BOUND ( 'NONE', #7491, .T. ) ;
#3069 = ORIENTED_EDGE ( 'NONE', *, *, #11678, .F. ) ;
#3070 = CARTESIAN_POINT ( 'NONE',  ( 0.000000000000000000, 1.178949249685218525, 2.041999999999999371 ) ) ;
#3071 = CARTESIAN_POINT ( 'NONE',  ( 0.000000000000000000, -13.85025647830069317, 17.79862902732260110 ) ) ;
#3072 = AXIS2_PLACEMENT_3D ( 'NONE', #4632, #4174, #7889 ) ;
#3073 = APPLICATION_CONTEXT ( 'automotive_design' ) ;
#3074 = ORIENTED_EDGE ( 'NONE', *, *, #11605, .F. ) ;
#3075 = ADVANCED_FACE ( 'NONE', ( #6966 ), #7967, .T. ) ;
#3076 = DIRECTION ( 'NONE',  ( 0.000000000000000000, 0.000000000000000000, -1.000000000000000000 ) ) ;
#3077 = DIRECTION ( 'NONE',  ( 0.000000000000000000, 0.3826834323650905589, -0.9238795325112864054 ) ) ;
#3078 = ORIENTED_EDGE ( 'NONE', *, *, #11451, .T. ) ;
#3079 = DIRECTION ( 'NONE',  ( 0.000000000000000000, 0.000000000000000000, -1.000000000000000000 ) ) ;
#3080 = FILL_AREA_STYLE ('',( #11624 ) ) ;
#3081 = FACE_OUTER_BOUND ( 'NONE', #4296, .T. ) ;
#3082 = DIRECTION ( 'NONE',  ( -1.000000000000000000, 0.000000000000000000, -0.000000000000000000 ) ) ;
#3083=STYLED_ITEM('',(#12398),#4318);
#3084 = VERTEX_POINT ( 'NONE', #4326 ) ;
#3085 = LINE ( 'NONE', #9764, #8389 ) ;
#3086 = DIRECTION ( 'NONE',  ( 0.000000000000000000, 0.6828850436591804574, 0.7305258497456468270 ) ) ;
#3087 = DIRECTION ( 'NONE',  ( 0.000000000000000000, 0.000000000000000000, 1.000000000000000000 ) ) ;
#3088 = CIRCLE ( 'NONE', #89, 3.873645755336797780 ) ;
#3089 = CARTESIAN_POINT ( 'NONE',  ( 0.000000000000000000, 0.000000000000000000, 0.000000000000000000 ) ) ;
#3090 = CYLINDRICAL_SURFACE ( 'NONE', #11035, 5.000000000000000000 ) ;
#3091 = EDGE_LOOP ( 'NONE', ( #9647, #7151, #8362, #1322 ) ) ;
#3092 = CARTESIAN_POINT ( 'NONE',  ( 4.999999999999999112, -26.33508479058324170, 5.955107813822415608 ) ) ;
#3093 = CARTESIAN_POINT ( 'NONE',  ( -15.00000000000000000, 40.00000000000000711, 0.000000000000000000 ) ) ;
#3094 = ORIENTED_EDGE ( 'NONE', *, *, #2896, .T. ) ;
#3095 = CARTESIAN_POINT ( 'NONE',  ( -26.00000000000000355, 0.000000000000000000, 0.000000000000000000 ) ) ;
#3096 = ORIENTED_EDGE ( 'NONE', *, *, #4781, .F. ) ;
#3097 = CYLINDRICAL_SURFACE ( 'NONE', #8835, 2.500000000000000444 ) ;
#3098 = AXIS2_PLACEMENT_3D ( 'NONE', #3766, #10579, #4898 ) ;
#3099 = EDGE_CURVE ( 'NONE', #5581, #12066, #6338, .T. ) ;
#3100 = DIRECTION ( 'NONE',  ( -1.000000000000000000, 0.000000000000000000, 0.000000000000000000 ) ) ;
#3101 = CARTESIAN_POINT ( 'NONE',  ( 36.00000000000000711, 9.184850993605149917E-16, 7.500000000000000888 ) ) ;
#3102 = EDGE_CURVE ( 'NONE', #11449, #138, #4644, .T. ) ;
#3103 = DIRECTION ( 'NONE',  ( 0.000000000000000000, -1.000000000000000000, 0.000000000000000000 ) ) ;
#3104 = LINE ( 'NONE', #1328, #4219 ) ;
#3105 = ORIENTED_EDGE ( 'NONE', *, *, #8754, .T. ) ;
#3106 = AXIS2_PLACEMENT_3D ( 'NONE', #1182, #6832, #5894 ) ;
#3107 = DIRECTION ( 'NONE',  ( -1.000000000000000000, 0.000000000000000000, 0.000000000000000000 ) ) ;
#3108 = ORIENTED_EDGE ( 'NONE', *, *, #10738, .T. ) ;
#3109 = DIRECTION ( 'NONE',  ( 0.000000000000000000, 1.224646799147353207E-16, 1.000000000000000000 ) ) ;
#3110 = CONTEXT_DEPENDENT_SHAPE_REPRESENTATION ( #4327, #2327 ) ;
#3111 = ORIENTED_EDGE ( 'NONE', *, *, #449, .F. ) ;
#3112 = ADVANCED_FACE ( 'NONE', ( #4517 ), #9105, .T. ) ;
#3113 = CARTESIAN_POINT ( 'NONE',  ( 4.999999999999999112, 0.000000000000000000, 0.000000000000000000 ) ) ;
#3114 = ORIENTED_EDGE ( 'NONE', *, *, #5318, .T. ) ;
#3115 = LINE ( 'NONE', #6801, #187 ) ;
#3116 = CARTESIAN_POINT ( 'NONE',  ( 0.000000000000000000, 21.74405275335758247, 15.58472803277463825 ) ) ;
#3117 = EDGE_CURVE ( 'NONE', #2097, #8354, #3445, .T. ) ;
#3118 = EDGE_CURVE ( 'NONE', #6551, #3276, #5437, .T. ) ;
#3119 = CARTESIAN_POINT ( 'NONE',  ( 0.000000000000000000, 0.000000000000000000, 0.000000000000000000 ) ) ;
#3121 = ADVANCED_FACE ( 'NONE', ( #11137 ), #3649, .F. ) ;
#3120 = CARTESIAN_POINT ( 'NONE',  ( -15.00000000000000000, 40.00000000000000711, 0.000000000000000000 ) ) ;
#3122 = ORIENTED_EDGE ( 'NONE', *, *, #1821, .F. ) ;
#3123 = EDGE_LOOP ( 'NONE', ( #5510, #11696, #8755, #10471 ) ) ;
#3124 = SURFACE_SIDE_STYLE ('',( #11718 ) ) ;
#3125 = ORIENTED_EDGE ( 'NONE', *, *, #8029, .T. ) ;
#3126 = CARTESIAN_POINT ( 'NONE',  ( 2.500000000000000000, 1.768423874527822681, -1.021000000000002794 ) ) ;
#3127 = ORIENTED_EDGE ( 'NONE', *, *, #12093, .T. ) ;
#3128 = LINE ( 'NONE', #1239, #8357 ) ;
#3129 = DIRECTION ( 'NONE',  ( 0.000000000000000000, 1.000000000000000000, -0.000000000000000000 ) ) ;
#3130 = PRODUCT_DEFINITION ( 'UNKNOWN', '', #10232, #9902 ) ;
#3131 = ORIENTED_EDGE ( 'NONE', *, *, #8782, .T. ) ;
#3132 = LINE ( 'NONE', #1428, #12137 ) ;
#3133 = CARTESIAN_POINT ( 'NONE',  ( 0.000000000000000000, 11.14352537685202016, -19.60720892790241265 ) ) ;
#3134 = EDGE_LOOP ( 'NONE', ( #5458, #4289, #2919, #11400 ) ) ;
#3135 = SURFACE_STYLE_FILL_AREA ( #2178 ) ;
#3136 =( NAMED_UNIT ( * ) SI_UNIT ( $, .STERADIAN. ) SOLID_ANGLE_UNIT ( ) );
#3137 = DIRECTION ( 'NONE',  ( -1.000000000000000000, 0.000000000000000000, 0.000000000000000000 ) ) ;
#3138 = CARTESIAN_POINT ( 'NONE',  ( 4.999999999999999112, 20.18872947935930995, 1.561154383803294410 ) ) ;
#3139 = VERTEX_POINT ( 'NONE', #12124 ) ;
#3140 = DIRECTION ( 'NONE',  ( 0.000000000000000000, 0.000000000000000000, 1.000000000000000000 ) ) ;
#3141 = EDGE_CURVE ( 'NONE', #9748, #114, #8250, .T. ) ;
#3142 = EDGE_CURVE ( 'NONE', #5656, #10139, #245, .T. ) ;
#3143 = CARTESIAN_POINT ( 'NONE',  ( 4.999999999999999112, 0.000000000000000000, 0.000000000000000000 ) ) ;
#3144 = LINE ( 'NONE', #1189, #11779 ) ;
#3145 = CYLINDRICAL_SURFACE ( 'NONE', #3858, 9.600000000009600853 ) ;
#3146 = LINE ( 'NONE', #4255, #1058 ) ;
#3147 = ORIENTED_EDGE ( 'NONE', *, *, #5391, .F. ) ;
#3148 = DIRECTION ( 'NONE',  ( 0.000000000000000000, 0.000000000000000000, -1.000000000000000000 ) ) ;
#3149 = DIRECTION ( 'NONE',  ( -1.000000000000000000, 0.000000000000000000, -0.000000000000000000 ) ) ;
#3150 = ORIENTED_EDGE ( 'NONE', *, *, #7887, .F. ) ;
#3151 = FACE_OUTER_BOUND ( 'NONE', #3282, .T. ) ;
#3152 = PRODUCT_DEFINITION_CONTEXT ( 'detailed design', #7311, 'design' ) ;
#3153 = ORIENTED_EDGE ( 'NONE', *, *, #3058, .F. ) ;
#3154 = CARTESIAN_POINT ( 'NONE',  ( 50.00005079999999680, 6.799999999999999822, 1.500000000000000000 ) ) ;
#3155 = FACE_OUTER_BOUND ( 'NONE', #4521, .T. ) ;
#3156 = CARTESIAN_POINT ( 'NONE',  ( -19.99999999999999645, 1.530808498934191521E-15, -12.50000000000000000 ) ) ;
#3157 = DIRECTION ( 'NONE',  ( -1.000000000000000000, -0.000000000000000000, -0.000000000000000000 ) ) ;
#3158 = DIRECTION ( 'NONE',  ( -0.000000000000000000, 1.000000000000000000, 0.000000000000000000 ) ) ;
#3159 = ORIENTED_EDGE ( 'NONE', *, *, #5852, .F. ) ;
#3160 = ORIENTED_EDGE ( 'NONE', *, *, #127, .T. ) ;
#3161 = SHAPE_DEFINITION_REPRESENTATION ( #2235, #11360 ) ;
#3162 = ORIENTED_EDGE ( 'NONE', *, *, #5155, .F. ) ;
#3163 = EDGE_CURVE ( 'NONE', #9430, #1491, #1522, .T. ) ;
#3164 = DIRECTION ( 'NONE',  ( -1.000000000000000000, -0.000000000000000000, -0.000000000000000000 ) ) ;
#3165 = ORIENTED_EDGE ( 'NONE', *, *, #8385, .T. ) ;
#3166 = DIRECTION ( 'NONE',  ( 1.000000000000000000, -0.000000000000000000, 0.000000000000000000 ) ) ;
#3167 = LINE ( 'NONE', #11773, #5201 ) ;
#3168 = CIRCLE ( 'NONE', #5156, 14.24900000001425049 ) ;
#3169 = FACE_OUTER_BOUND ( 'NONE', #165, .T. ) ;
#3170 = FACE_OUTER_BOUND ( 'NONE', #9688, .T. ) ;
#3171 = ORIENTED_EDGE ( 'NONE', *, *, #1570, .F. ) ;
#3172 = ORIENTED_EDGE ( 'NONE', *, *, #1649, .T. ) ;
#3173 = ADVANCED_FACE ( 'NONE', ( #2641 ), #516, .T. ) ;
#3174 = PRESENTATION_STYLE_ASSIGNMENT (( #2230 ) ) ;
#3175 = ORIENTED_EDGE ( 'NONE', *, *, #9835, .T. ) ;
#3177 = CARTESIAN_POINT ( 'NONE',  ( 51.00000000000000000, 3.500000000000001332, -38.49999999999998579 ) ) ;
#3176 = CIRCLE ( 'NONE', #6764, 40.00000000000000711 ) ;
#3178 = AXIS2_PLACEMENT_3D ( 'NONE', #8076, #11620, #6065 ) ;
#3179 = EDGE_CURVE ( 'NONE', #11480, #2942, #2047, .T. ) ;
#3180 = DIRECTION ( 'NONE',  ( -1.000000000000000000, -0.000000000000000000, -0.000000000000000000 ) ) ;
#3181 = EDGE_CURVE ( 'NONE', #12228, #7460, #11083, .T. ) ;
#3182 = CARTESIAN_POINT ( 'NONE',  ( 37.00000000000000711, 0.000000000000000000, 1.500000000000000000 ) ) ;
#3183 = AXIS2_PLACEMENT_3D ( 'NONE', #1863, #9492, #4674 ) ;
#3184 = ORIENTED_EDGE ( 'NONE', *, *, #4023, .F. ) ;
#3185 = VECTOR ( 'NONE', #11275, 1000.000000000000000 ) ;
#3186 = DIRECTION ( 'NONE',  ( 0.03086419753086420623, 0.9995235871707959241, -0.000000000000000000 ) ) ;
#3187 = VERTEX_POINT ( 'NONE', #4386 ) ;
#3188 = CARTESIAN_POINT ( 'NONE',  ( 43.00000000000000000, -3.058102613202345665, 3.699730856038719207 ) ) ;
#3189 =( NAMED_UNIT ( * ) SI_UNIT ( $, .STERADIAN. ) SOLID_ANGLE_UNIT ( ) );
#3190 = CARTESIAN_POINT ( 'NONE',  ( -33.00000000000000000, -7.960204194457796463E-16, -6.500000000000000888 ) ) ;
#3191 = DIRECTION ( 'NONE',  ( 0.000000000000000000, 0.4999999999999993339, -0.8660254037844390407 ) ) ;
#3192 = EDGE_CURVE ( 'NONE', #6862, #8676, #704, .T. ) ;
#3193 = VERTEX_POINT ( 'NONE', #7288 ) ;
#3194 = DIRECTION ( 'NONE',  ( 0.000000000000000000, 1.000000000000000000, 0.000000000000000000 ) ) ;
#3195 = EDGE_CURVE ( 'NONE', #9779, #5745, #641, .T. ) ;
#3196 = AXIS2_PLACEMENT_3D ( 'NONE', #1013, #4706, #8471 ) ;
#3197 = CIRCLE ( 'NONE', #7990, 14.24900000001425404 ) ;
#3198 = DIRECTION ( 'NONE',  ( 0.000000000000000000, 1.224646799147343593E-16, 1.000000000000000000 ) ) ;
#3199 = DIRECTION ( 'NONE',  ( -1.000000000000000000, 0.000000000000000000, 0.000000000000000000 ) ) ;
#3200 = CARTESIAN_POINT ( 'NONE',  ( 0.000000000000000000, 1.178949249685213863, -2.042000000000001148 ) ) ;
#3201 = CARTESIAN_POINT ( 'NONE',  ( 42.00000000000000000, 6.799999999999998046, -1.500000000000000000 ) ) ;
#3202 = DIRECTION ( 'NONE',  ( -1.000000000000000000, 0.000000000000000000, -0.000000000000000000 ) ) ;
#3203 = VECTOR ( 'NONE', #10398, 1000.000000000000000 ) ;
#3204 = ORIENTED_EDGE ( 'NONE', *, *, #5271, .F. ) ;
#3205 = ORIENTED_EDGE ( 'NONE', *, *, #4499, .T. ) ;
#3206 = CYLINDRICAL_SURFACE ( 'NONE', #1185, 20.24900000002024569 ) ;
#3207 = EDGE_CURVE ( 'NONE', #2267, #4122, #3466, .T. ) ;
#3208 = DIRECTION ( 'NONE',  ( 1.000000000000000000, 0.000000000000000000, 0.000000000000000000 ) ) ;
#3209 = ADVANCED_FACE ( 'NONE', ( #7468 ), #11264, .T. ) ;
#3210 =( GEOMETRIC_REPRESENTATION_CONTEXT ( 3 ) GLOBAL_UNCERTAINTY_ASSIGNED_CONTEXT ( ( #7792 ) ) GLOBAL_UNIT_ASSIGNED_CONTEXT ( ( #10329, #3718, #7530 ) ) REPRESENTATION_CONTEXT ( 'NONE', 'WORKASPACE' ) );
#3211 = ORIENTED_EDGE ( 'NONE', *, *, #12328, .F. ) ;
#3212 = DIRECTION ( 'NONE',  ( 0.000000000000000000, -0.000000000000000000, -1.000000000000000000 ) ) ;
#3213 = ORIENTED_EDGE ( 'NONE', *, *, #9033, .F. ) ;
#3214 = LINE ( 'NONE', #9955, #7837 ) ;
#3215 = AXIS2_PLACEMENT_3D ( 'NONE', #9393, #3462, #750 ) ;
#3216 = VECTOR ( 'NONE', #6013, 1000.000000000000000 ) ;
#3217 = TOROIDAL_SURFACE ( 'NONE', #1398, 4.000000000000000000, 0.2500000000000000000 ) ;
#3218 = CARTESIAN_POINT ( 'NONE',  ( 45.00000000000000000, 6.123233995736765296E-16, -5.000000000000000000 ) ) ;
#3219 = DIRECTION ( 'NONE',  ( -1.000000000000000000, -0.000000000000000000, 0.000000000000000000 ) ) ;
#3220 = DIRECTION ( 'NONE',  ( 0.000000000000000000, -0.8660254037844432595, 0.4999999999999920619 ) ) ;
#3221 = ORIENTED_EDGE ( 'NONE', *, *, #6575, .T. ) ;
#3222 = AXIS2_PLACEMENT_3D ( 'NONE', #1893, #3757, #4943 ) ;
#3223 = ORIENTED_EDGE ( 'NONE', *, *, #9680, .T. ) ;
#3224 = DIRECTION ( 'NONE',  ( 0.000000000000000000, 0.8660254037844380415, -0.5000000000000011102 ) ) ;
#3225 = ORIENTED_EDGE ( 'NONE', *, *, #2636, .T. ) ;
#3226 = AXIS2_PLACEMENT_3D ( 'NONE', #6049, #291, #4105 ) ;
#3227 = APPLICATION_CONTEXT ( 'automotive_design' ) ;
#3228 = CARTESIAN_POINT ( 'NONE',  ( 26.00000000000000355, 30.00000000000000711, -19.99999999999998934 ) ) ;
#3229 = MECHANICAL_DESIGN_GEOMETRIC_PRESENTATION_REPRESENTATION (  '', ( #4626 ), #7027 ) ;
#3230 = AXIS2_PLACEMENT_3D ( 'NONE', #10540, #5047, #4794 ) ;
#3231 = AXIS2_PLACEMENT_3D ( 'NONE', #4896, #6847, #2022 ) ;
#3232 = DIRECTION ( 'NONE',  ( 0.000000000000000000, 0.000000000000000000, 1.000000000000000000 ) ) ;
#3233 = LINE ( 'NONE', #10784, #10005 ) ;
#3234 = VECTOR ( 'NONE', #9728, 1000.000000000000000 ) ;
#3235 = CARTESIAN_POINT ( 'NONE',  ( 2.500000000000000000, 0.000000000000000000, 0.000000000000000000 ) ) ;
#3236 = DIRECTION ( 'NONE',  ( -1.000000000000000000, -0.000000000000000000, 0.000000000000000000 ) ) ;
#3237 = EDGE_LOOP ( 'NONE', ( #729, #6792, #12079, #12349 ) ) ;
#3238 = CYLINDRICAL_SURFACE ( 'NONE', #11617, 12.49999999999999645 ) ;
#3239 = ORIENTED_EDGE ( 'NONE', *, *, #6313, .F. ) ;
#3240 =( LENGTH_UNIT ( ) NAMED_UNIT ( * ) SI_UNIT ( .MILLI., .METRE. ) );
#3241 = EDGE_LOOP ( 'NONE', ( #6976, #6122 ) ) ;
#3242 = STYLED_ITEM ( 'NONE', ( #10987 ), #6615 ) ;
#3243 = CONICAL_SURFACE ( 'NONE', #36, 2.500000000000002220, 1.029744260000000189 ) ;
#3244 = DIRECTION ( 'NONE',  ( -1.000000000000000000, -0.000000000000000000, -0.000000000000000000 ) ) ;
#3245 = CIRCLE ( 'NONE', #9639, 9.600000000009599077 ) ;
#3246 = PRODUCT_DEFINITION_SHAPE ( 'NONE', 'NONE',  #12370 ) ;
#3247 = AXIS2_PLACEMENT_3D ( 'NONE', #9580, #8711, #7659 ) ;
#3248 = LINE ( 'NONE', #7993, #12129 ) ;
#3249 = DIRECTION ( 'NONE',  ( 0.000000000000000000, 0.000000000000000000, 1.000000000000000000 ) ) ;
#3250 = EDGE_CURVE ( 'NONE', #102, #3326, #5640, .T. ) ;
#3251 = PRODUCT_DEFINITION_FORMATION_WITH_SPECIFIED_SOURCE ( 'ANY', '', #6836, .NOT_KNOWN. ) ;
#3252 = CIRCLE ( 'NONE', #11021, 0.1000000000000002554 ) ;
#3253 = VECTOR ( 'NONE', #1483, 1000.000000000000000 ) ;
#3254 = EDGE_CURVE ( 'NONE', #5033, #4657, #3760, .T. ) ;
#3255 = ORIENTED_EDGE ( 'NONE', *, *, #9698, .F. ) ;
#3256 = AXIS2_PLACEMENT_3D ( 'NONE', #4077, #9716, #5189 ) ;
#3257 = DIRECTION ( 'NONE',  ( 0.000000000000000000, -0.5000000000000011102, -0.8660254037844379305 ) ) ;
#3258 = ORIENTED_EDGE ( 'NONE', *, *, #1462, .F. ) ;
#3259 = CARTESIAN_POINT ( 'NONE',  ( 4.999999999999999112, 8.035066368449411911, -14.88411597386720508 ) ) ;
#3260 = CARTESIAN_POINT ( 'NONE',  ( 4.999999999999999112, 0.4834863907628118573, -16.90755573046745397 ) ) ;
#3261 = LINE ( 'NONE', #3138, #7495 ) ;
#3262 = ORIENTED_EDGE ( 'NONE', *, *, #7381, .F. ) ;
#3263 = DIRECTION ( 'NONE',  ( -1.000000000000000000, -0.000000000000000000, -0.000000000000000000 ) ) ;
#3264 = VECTOR ( 'NONE', #4703, 1000.000000000000000 ) ;
#3265 = AXIS2_PLACEMENT_3D ( 'NONE', #2244, #7818, #3077 ) ;
#3266 = CARTESIAN_POINT ( 'NONE',  ( 50.00005079999999680, 6.799999999999999822, -1.500000000000000000 ) ) ;
#3267 = EDGE_CURVE ( 'NONE', #8693, #3572, #137, .T. ) ;
#3268 = CARTESIAN_POINT ( 'NONE',  ( -20.63749999999999929, 0.000000000000000000, -5.750000000000000000 ) ) ;
#3269 = DIRECTION ( 'NONE',  ( -1.000000000000000000, 0.000000000000000000, 0.000000000000000000 ) ) ;
#3270 = EDGE_CURVE ( 'NONE', #1899, #10913, #3641, .T. ) ;
#3271 = ADVANCED_FACE ( 'NONE', ( #11559, #944 ), #6580, .T. ) ;
#3272 = CARTESIAN_POINT ( 'NONE',  ( 4.999999999999999112, 19.24938187143305512, -6.283573709965099674 ) ) ;
#3273 = DIRECTION ( 'NONE',  ( 1.000000000000000000, -0.000000000000000000, -0.000000000000000000 ) ) ;
#3274 = ADVANCED_FACE ( 'NONE', ( #10571 ), #2018, .F. ) ;
#3275 = ORIENTED_EDGE ( 'NONE', *, *, #10679, .T. ) ;
#3276 = VERTEX_POINT ( 'NONE', #12256 ) ;
#3277 = DIRECTION ( 'NONE',  ( -1.000000000000000000, 0.000000000000000000, 0.000000000000000000 ) ) ;
#3278 = CIRCLE ( 'NONE', #5474, 7.500000000000000000 ) ;
#3279 = CARTESIAN_POINT ( 'NONE',  ( 1.399999999999998579, 9.184850993605147944E-16, 7.500000000000000000 ) ) ;
#3280 = VERTEX_POINT ( 'NONE', #8469 ) ;
#3281 = CARTESIAN_POINT ( 'NONE',  ( 4.999999999999999112, -22.37914155802283034, -2.791921004064479739 ) ) ;
#3282 = EDGE_LOOP ( 'NONE', ( #9061, #8705, #2213, #3750 ) ) ;
#3283 = CARTESIAN_POINT ( 'NONE',  ( 4.999999999999999112, 13.09267581720874674, -5.622796541391427816 ) ) ;
#3284 = ADVANCED_FACE ( 'NONE', ( #5646 ), #9469, .T. ) ;
#3285 = AXIS2_PLACEMENT_3D ( 'NONE', #2577, #6288, #5402 ) ;
#3286 = DIRECTION ( 'NONE',  ( -1.000000000000000000, 0.000000000000000000, 0.000000000000000000 ) ) ;
#3287 = DIRECTION ( 'NONE',  ( 0.000000000000000000, 0.000000000000000000, -1.000000000000000000 ) ) ;
#3288 = DIRECTION ( 'NONE',  ( -1.000000000000000000, 0.000000000000000000, 0.000000000000000000 ) ) ;
#3289 = ORIENTED_EDGE ( 'NONE', *, *, #3043, .F. ) ;
#3290 = CARTESIAN_POINT ( 'NONE',  ( -20.63749999999999574, 8.266365894244634333E-16, 6.750000000000000000 ) ) ;
#3291 = EDGE_LOOP ( 'NONE', ( #5014, #12285, #7753, #4819 ) ) ;
#3292 = DIRECTION ( 'NONE',  ( 1.000000000000000000, 0.000000000000000000, 0.000000000000000000 ) ) ;
#3293 = ORIENTED_EDGE ( 'NONE', *, *, #11266, .T. ) ;
#3294 = EDGE_CURVE ( 'NONE', #2779, #4243, #891, .T. ) ;
#3295 = ORIENTED_EDGE ( 'NONE', *, *, #4779, .F. ) ;
#3296 = EDGE_CURVE ( 'NONE', #7220, #10481, #11427, .T. ) ;
#3297 = DIRECTION ( 'NONE',  ( -0.000000000000000000, 1.000000000000000000, 0.000000000000000000 ) ) ;
#3298 = LINE ( 'NONE', #6293, #9608 ) ;
#3299 = AXIS2_PLACEMENT_3D ( 'NONE', #650, #10326, #2520 ) ;
#3300 = DIRECTION ( 'NONE',  ( 0.000000000000000000, 0.000000000000000000, -1.000000000000000000 ) ) ;
#3301 = CARTESIAN_POINT ( 'NONE',  ( 0.000000000000000000, 11.14352537685174660, 19.60720892790256897 ) ) ;
#3302 = ORIENTED_EDGE ( 'NONE', *, *, #10428, .T. ) ;
#3303 = CARTESIAN_POINT ( 'NONE',  ( 42.00000000000000000, 0.000000000000000000, 0.000000000000000000 ) ) ;
#3304 = EDGE_LOOP ( 'NONE', ( #3868, #3993, #10667, #2954 ) ) ;
#3305 = CARTESIAN_POINT ( 'NONE',  ( 0.000000000000000000, 0.000000000000000000, 0.000000000000000000 ) ) ;
#3306 = ORIENTED_EDGE ( 'NONE', *, *, #4739, .T. ) ;
#3307 = CYLINDRICAL_SURFACE ( 'NONE', #1228, 5.999999999999999112 ) ;
#3308 = APPLICATION_CONTEXT ( 'automotive_design' ) ;
#3309 = AXIS2_PLACEMENT_3D ( 'NONE', #2508, #6330, #1696 ) ;
#3310 = CARTESIAN_POINT ( 'NONE',  ( -15.00000000000000000, 44.00000000000001421, 0.000000000000000000 ) ) ;
#3311 = DIRECTION ( 'NONE',  ( -1.000000000000000000, 0.000000000000000000, 0.000000000000000000 ) ) ;
#3312 = ORIENTED_EDGE ( 'NONE', *, *, #3005, .T. ) ;
#3313 = CARTESIAN_POINT ( 'NONE',  ( 0.000000000000000000, -19.24938187143300539, 6.283573709965241783 ) ) ;
#3314 = EDGE_LOOP ( 'NONE', ( #163, #7537, #2905, #8145, #10230 ) ) ;
#3315 = CARTESIAN_POINT ( 'NONE',  ( 4.999999999999999112, -17.79862902732275032, 13.85025647830051021 ) ) ;
#3316 = DIRECTION ( 'NONE',  ( 0.000000000000000000, 0.000000000000000000, 1.000000000000000000 ) ) ;
#3317 = EDGE_CURVE ( 'NONE', #10227, #9587, #6046, .T. ) ;
#3318 = ORIENTED_EDGE ( 'NONE', *, *, #8595, .F. ) ;
#3319 = CARTESIAN_POINT ( 'NONE',  ( 2.499999999999999556, 20.13931372320388391, 5.950465759858938775 ) ) ;
#3320 = ADVANCED_FACE ( 'NONE', ( #7522 ), #9238, .F. ) ;
#3321 = PLANE ( 'NONE',  #5184 ) ;
#3322 = CARTESIAN_POINT ( 'NONE',  ( 37.00000000000000711, 1.456773409934505593E-31, -41.99999999999998579 ) ) ;
#3323 = DIRECTION ( 'NONE',  ( 0.000000000000000000, 2.664535259100374514E-15, 1.000000000000000000 ) ) ;
#3324 = DIRECTION ( 'NONE',  ( -1.000000000000000000, 0.000000000000000000, -0.000000000000000000 ) ) ;
#3325 = CARTESIAN_POINT ( 'NONE',  ( 26.00000000000000355, 30.00000000000000711, 0.000000000000000000 ) ) ;
#3326 = VERTEX_POINT ( 'NONE', #2755 ) ;
#3327 = ORIENTED_EDGE ( 'NONE', *, *, #658, .F. ) ;
#3328 = CARTESIAN_POINT ( 'NONE',  ( 15.00000000000000355, 30.00000000000000711, 0.000000000000000000 ) ) ;
#3329 = CARTESIAN_POINT ( 'NONE',  ( 0.000000000000000000, 0.000000000000000000, 0.000000000000000000 ) ) ;
#3330 = ORIENTED_EDGE ( 'NONE', *, *, #5386, .T. ) ;
#3331 = CARTESIAN_POINT ( 'NONE',  ( 33.00000000000000000, 9.184850993605147944E-16, -34.49999999999999289 ) ) ;
#3332 = EDGE_CURVE ( 'NONE', #4444, #4464, #4759, .T. ) ;
#3333 = ORIENTED_EDGE ( 'NONE', *, *, #11274, .F. ) ;
#3334 = CARTESIAN_POINT ( 'NONE',  ( 36.00000000000000711, 9.184850993605147944E-16, -34.49999999999999289 ) ) ;
#3335 = ADVANCED_FACE ( 'NONE', ( #11382 ), #6, .T. ) ;
#3336 = EDGE_CURVE ( 'NONE', #5455, #12039, #2898, .T. ) ;
#3337 = SURFACE_STYLE_USAGE ( .BOTH. , #9857 ) ;
#3338 = DIRECTION ( 'NONE',  ( 0.000000000000000000, -1.000000000000000000, -1.047444401652940007E-14 ) ) ;
#3339 = CARTESIAN_POINT ( 'NONE',  ( 4.999999999999999112, -8.035066368449101049, -14.88411597386737562 ) ) ;
#3340 = DIRECTION ( 'NONE',  ( -1.000000000000000000, -0.000000000000000000, 0.000000000000000000 ) ) ;
#3341 = ORIENTED_EDGE ( 'NONE', *, *, #3710, .F. ) ;
#3342 = DIRECTION ( 'NONE',  ( 0.000000000000000000, 0.5068368027542901055, -0.8620420264545163302 ) ) ;
#3343 = LINE ( 'NONE', #10039, #5212 ) ;
#3344 = ORIENTED_EDGE ( 'NONE', *, *, #6728, .F. ) ;
#3345 = PRESENTATION_STYLE_ASSIGNMENT (( #9050 ) ) ;
#3346 = ORIENTED_EDGE ( 'NONE', *, *, #593, .F. ) ;
#3347 = CARTESIAN_POINT ( 'NONE',  ( -0.5590169943749470072, 7.041719095097280880E-16, 5.750000000000000000 ) ) ;
#3348 = FACE_OUTER_BOUND ( 'NONE', #7452, .T. ) ;
#3349 = CARTESIAN_POINT ( 'NONE',  ( 65.79898987322334847, 7.000000000000004441, -41.99999999999998579 ) ) ;
#3350 = ORIENTED_EDGE ( 'NONE', *, *, #12172, .T. ) ;
#3351 = LINE ( 'NONE', #2292, #8646 ) ;
#3352 = ORIENTED_EDGE ( 'NONE', *, *, #1317, .T. ) ;
#3353 = DIRECTION ( 'NONE',  ( 0.000000000000000000, -0.9242245927363030855, -0.3818493186865927203 ) ) ;
#3354 = ADVANCED_FACE ( 'NONE', ( #10648 ), #6769, .T. ) ;
#3356 = EDGE_CURVE ( 'NONE', #8297, #5359, #10222, .T. ) ;
#3355 = VERTEX_POINT ( 'NONE', #3897 ) ;
#3357 = LINE ( 'NONE', #7250, #9617 ) ;
#3358 = CARTESIAN_POINT ( 'NONE',  ( 51.00000000000000000, 3.061616997868380183E-16, -39.49999999999999289 ) ) ;
#3359 = VERTEX_POINT ( 'NONE', #5574 ) ;
#3360 = DIRECTION ( 'NONE',  ( 0.000000000000000000, 0.000000000000000000, 1.000000000000000000 ) ) ;
#3361 = VERTEX_POINT ( 'NONE', #9398 ) ;
#3362 = CARTESIAN_POINT ( 'NONE',  ( -0.5000000000000000000, -6.429618962271402616, -1.000000000000000000 ) ) ;
#3363 = AXIS2_PLACEMENT_3D ( 'NONE', #3808, #4743, #4873 ) ;
#3364 = ORIENTED_EDGE ( 'NONE', *, *, #6575, .F. ) ;
#3365 = VECTOR ( 'NONE', #11829, 1000.000000000000000 ) ;
#3366 = FACE_OUTER_BOUND ( 'NONE', #11200, .T. ) ;
#3367 = ORIENTED_EDGE ( 'NONE', *, *, #74, .T. ) ;
#3368 = CARTESIAN_POINT ( 'NONE',  ( 0.000000000000000000, 0.000000000000000000, 0.000000000000000000 ) ) ;
#3369 = VECTOR ( 'NONE', #8356, 1000.000000000000000 ) ;
#3370 = CIRCLE ( 'NONE', #9378, 7.200000000007201528 ) ;
#3371 = DIRECTION ( 'NONE',  ( -1.000000000000000000, 0.000000000000000000, 0.000000000000000000 ) ) ;
#3372 = CARTESIAN_POINT ( 'NONE',  ( 1.000000000000000000, 0.5999999999999998668, 3.826895796574397046 ) ) ;
#3373 = CARTESIAN_POINT ( 'NONE',  ( 24.00000000000000000, 0.000000000000000000, -48.00000000000000000 ) ) ;
#3374 = FACE_BOUND ( 'NONE', #12099, .T. ) ;
#3375 = DIRECTION ( 'NONE',  ( -1.000000000000000000, -0.000000000000000000, 0.000000000000000000 ) ) ;
#3376 = VERTEX_POINT ( 'NONE', #7017 ) ;
#3377 = ORIENTED_EDGE ( 'NONE', *, *, #3390, .T. ) ;
#3378 = DIRECTION ( 'NONE',  ( -1.000000000000000000, 4.770489558936236458E-18, 0.000000000000000000 ) ) ;
#3379 = DIRECTION ( 'NONE',  ( 0.000000000000000000, 0.000000000000000000, -1.000000000000000000 ) ) ;
#3380 = CIRCLE ( 'NONE', #8583, 14.24900000001425227 ) ;
#3381 = ORIENTED_EDGE ( 'NONE', *, *, #9150, .F. ) ;
#3382 = DIRECTION ( 'NONE',  ( -1.000000000000000000, 0.000000000000000000, 0.000000000000000000 ) ) ;
#3383 = AXIS2_PLACEMENT_3D ( 'NONE', #3368, #1618, #4497 ) ;
#3384 = EDGE_LOOP ( 'NONE', ( #6916, #11579, #5274, #3074, #7548, #5520, #3726, #2649 ) ) ;
#3385 = CARTESIAN_POINT ( 'NONE',  ( 2.500000000000000000, 2.357898499370433054, -1.951563910473907981E-15 ) ) ;
#3386 = VECTOR ( 'NONE', #11710, 1000.000000000000114 ) ;
#3387 = EDGE_LOOP ( 'NONE', ( #10721, #8540, #10310, #7323 ) ) ;
#3388 =( NAMED_UNIT ( * ) SI_UNIT ( $, .STERADIAN. ) SOLID_ANGLE_UNIT ( ) );
#3389 = DIRECTION ( 'NONE',  ( 0.000000000000000000, 0.000000000000000000, 1.000000000000000000 ) ) ;
#3390 = EDGE_CURVE ( 'NONE', #10829, #420, #9022, .T. ) ;
#3391 = AXIS2_PLACEMENT_3D ( 'NONE', #6076, #4128, #9084 ) ;
#3392 = DIRECTION ( 'NONE',  ( 1.000000000000000000, 0.000000000000000000, 0.000000000000000000 ) ) ;
#3393 = CARTESIAN_POINT ( 'NONE',  ( 4.999999999999999112, 1.561154383803221579, 20.18872947935931705 ) ) ;
#3394 = EDGE_LOOP ( 'NONE', ( #10298, #8483, #1515, #2702 ) ) ;
#3395 = EDGE_CURVE ( 'NONE', #1109, #1723, #11810, .T. ) ;
#3396 = DIRECTION ( 'NONE',  ( 1.000000000000000000, 0.000000000000000000, 0.000000000000000000 ) ) ;
#3397 = DIRECTION ( 'NONE',  ( -1.000000000000000000, -0.000000000000000000, -0.000000000000000000 ) ) ;
#3398 = ORIENTED_EDGE ( 'NONE', *, *, #11192, .F. ) ;
#3399 = DIRECTION ( 'NONE',  ( 0.000000000000000000, -0.3826834323650971093, 0.9238795325112837409 ) ) ;
#3400 = CONTEXT_DEPENDENT_SHAPE_REPRESENTATION ( #6669, #9045 ) ;
#3401 = VERTEX_POINT ( 'NONE', #8954 ) ;
#3402 = VECTOR ( 'NONE', #2781, 1000.000000000000000 ) ;
#3403 = AXIS2_PLACEMENT_3D ( 'NONE', #11542, #10552, #4807 ) ;
#3404 = CARTESIAN_POINT ( 'NONE',  ( 4.999999999999999112, -9.168210874537708222, 18.05452603534162748 ) ) ;
#3405 = FACE_OUTER_BOUND ( 'NONE', #5536, .T. ) ;
#3406 = CARTESIAN_POINT ( 'NONE',  ( 4.999999999999999112, -22.37914155802283034, -2.791921004064479739 ) ) ;
#3407 = DIRECTION ( 'NONE',  ( -1.000000000000000000, 0.000000000000000000, 0.000000000000000000 ) ) ;
#3408 = DIRECTION ( 'NONE',  ( -1.000000000000000000, 4.770489558936236458E-18, -6.855277276495154548E-34 ) ) ;
#3409 = AXIS2_PLACEMENT_3D ( 'NONE', #9944, #7133, #10822 ) ;
#3410 = VERTEX_POINT ( 'NONE', #2193 ) ;
#3411 = EDGE_CURVE ( 'NONE', #103, #2147, #5129, .T. ) ;
#3412 = CIRCLE ( 'NONE', #7005, 0.7500000000000000000 ) ;
#3413 = EDGE_CURVE ( 'NONE', #10829, #185, #10631, .T. ) ;
#3414 = DIRECTION ( 'NONE',  ( 0.000000000000000000, 0.000000000000000000, -1.000000000000000000 ) ) ;
#3415 = CIRCLE ( 'NONE', #2016, 14.24900000001425049 ) ;
#3416 = ADVANCED_FACE ( 'NONE', ( #9894 ), #5953, .F. ) ;
#3417 = VERTEX_POINT ( 'NONE', #7841 ) ;
#3418 = PRESENTATION_STYLE_ASSIGNMENT (( #1598 ) ) ;
#3419 = ORIENTED_EDGE ( 'NONE', *, *, #4699, .T. ) ;
#3420 = DIRECTION ( 'NONE',  ( -1.000000000000000000, -0.000000000000000000, -0.000000000000000000 ) ) ;
#3421 = DIRECTION ( 'NONE',  ( 1.000000000000000000, 0.000000000000000000, 0.000000000000000000 ) ) ;
#3422 = AXIS2_PLACEMENT_3D ( 'NONE', #2923, #5980, #5926 ) ;
#3423 = AXIS2_PLACEMENT_3D ( 'NONE', #7291, #1110, #4922 ) ;
#3424 = AXIS2_PLACEMENT_3D ( 'NONE', #12031, #10106, #1592 ) ;
#3425 = CIRCLE ( 'NONE', #5619, 21.00000000002100009 ) ;
#3426 = ORIENTED_EDGE ( 'NONE', *, *, #4164, .T. ) ;
#3427 = DIRECTION ( 'NONE',  ( 1.000000000000000000, 0.000000000000000000, 0.000000000000000000 ) ) ;
#3428 = EDGE_CURVE ( 'NONE', #9779, #2502, #3146, .T. ) ;
#3429 = ORIENTED_EDGE ( 'NONE', *, *, #11974, .F. ) ;
#3430 = DIRECTION ( 'NONE',  ( 0.000000000000000000, -0.9238795325112826307, -0.3826834323650997183 ) ) ;
#3431 = CIRCLE ( 'NONE', #2632, 9.600000000009600853 ) ;
#3432 = ORIENTED_EDGE ( 'NONE', *, *, #11724, .T. ) ;
#3433 = VECTOR ( 'NONE', #7088, 1000.000000000000000 ) ;
#3434 = VECTOR ( 'NONE', #6861, 1000.000000000000000 ) ;
#3435 = AXIS2_PLACEMENT_3D ( 'NONE', #630, #4512, #9391 ) ;
#3436 = DIRECTION ( 'NONE',  ( 0.000000000000000000, 0.000000000000000000, 1.000000000000000000 ) ) ;
#3437 = ORIENTED_EDGE ( 'NONE', *, *, #11603, .F. ) ;
#3438 = DIRECTION ( 'NONE',  ( 0.000000000000000000, 0.000000000000000000, 1.000000000000000000 ) ) ;
#3439 = MECHANICAL_DESIGN_GEOMETRIC_PRESENTATION_REPRESENTATION (  '', ( #639 ), #7248 ) ;
#3440 = AXIS2_PLACEMENT_3D ( 'NONE', #4459, #4385, #1704 ) ;
#3441 = AXIS2_PLACEMENT_3D ( 'NONE', #6123, #1306, #5120 ) ;
#3442 = PRODUCT_DEFINITION_SHAPE ( 'NONE', 'NONE',  #12361 ) ;
#3443 = CARTESIAN_POINT ( 'NONE',  ( 1.399999999999999689, 9.062386313690412402E-16, 7.399999999999999467 ) ) ;
#3444 = EDGE_CURVE ( 'NONE', #9643, #12234, #11814, .T. ) ;
#3445 = CIRCLE ( 'NONE', #6654, 5.000000000000000000 ) ;
#3446 = CARTESIAN_POINT ( 'NONE',  ( 46.00000000000000000, 1.456773409934505593E-31, -36.99999999999998579 ) ) ;
#3447 = FACE_BOUND ( 'NONE', #1916, .T. ) ;
#3448 = FACE_OUTER_BOUND ( 'NONE', #5110, .T. ) ;
#3449 = LINE ( 'NONE', #4308, #1862 ) ;
#3450 = VERTEX_POINT ( 'NONE', #2082 ) ;
#3451 = ORIENTED_EDGE ( 'NONE', *, *, #2333, .T. ) ;
#3452 = FACE_OUTER_BOUND ( 'NONE', #892, .T. ) ;
#3453 = SURFACE_SIDE_STYLE ('',( #506 ) ) ;
#3454 = DIRECTION ( 'NONE',  ( 0.000000000000000000, 0.000000000000000000, 1.000000000000000000 ) ) ;
#3455 = AXIS2_PLACEMENT_3D ( 'NONE', #8022, #11001, #10931 ) ;
#3456 = ORIENTED_EDGE ( 'NONE', *, *, #283, .T. ) ;
#3457 = CARTESIAN_POINT ( 'NONE',  ( 4.999999999999999112, 11.14352537685174660, 19.60720892790256897 ) ) ;
#3458 = VECTOR ( 'NONE', #12276, 1000.000000000000000 ) ;
#3459 = VECTOR ( 'NONE', #1882, 1000.000000000000000 ) ;
#3460 = VERTEX_POINT ( 'NONE', #1371 ) ;
#3461 = DIRECTION ( 'NONE',  ( 1.000000000000000000, 0.000000000000000000, 0.000000000000000000 ) ) ;
#3462 = DIRECTION ( 'NONE',  ( -1.000000000000000000, 0.000000000000000000, 0.000000000000000000 ) ) ;
#3463 = CYLINDRICAL_SURFACE ( 'NONE', #4356, 7.200000000007202416 ) ;
#3464 = AXIS2_PLACEMENT_3D ( 'NONE', #9092, #8273, #9143 ) ;
#3465 = FACE_OUTER_BOUND ( 'NONE', #1315, .T. ) ;
#3466 = LINE ( 'NONE', #8401, #7253 ) ;
#3467 =( REPRESENTATION_RELATIONSHIP ('NONE','NONE', #9709, #7217 ) REPRESENTATION_RELATIONSHIP_WITH_TRANSFORMATION ( #9794 )SHAPE_REPRESENTATION_RELATIONSHIP( ) );
#3468 = ORIENTED_EDGE ( 'NONE', *, *, #2140, .T. ) ;
#3469 = FACE_OUTER_BOUND ( 'NONE', #6698, .T. ) ;
#3470 = CARTESIAN_POINT ( 'NONE',  ( 4.999999999999999112, -6.283573709965446064, 19.24938187143294144 ) ) ;
#3471 = ORIENTED_EDGE ( 'NONE', *, *, #1256, .F. ) ;
#3472 = DIRECTION ( 'NONE',  ( -1.000000000000000000, 0.000000000000000000, 0.000000000000000000 ) ) ;
#3473 = CONTEXT_DEPENDENT_SHAPE_REPRESENTATION ( #10950, #5124 ) ;
#3474 = ORIENTED_EDGE ( 'NONE', *, *, #5702, .T. ) ;
#3475 = ADVANCED_FACE ( 'NONE', ( #2312 ), #6132, .T. ) ;
#3476 = EDGE_CURVE ( 'NONE', #11705, #7774, #8839, .T. ) ;
#3477 = CARTESIAN_POINT ( 'NONE',  ( -33.00000000000000000, -9.184850993605149917E-16, 7.500000000000000888 ) ) ;
#3478 = LINE ( 'NONE', #2769, #3990 ) ;
#3479 = FACE_OUTER_BOUND ( 'NONE', #9340, .T. ) ;
#3480 = CARTESIAN_POINT ( 'NONE',  ( -36.00000000000000711, -4.898587196589413815E-15, -40.00000000000000711 ) ) ;
#3481 = DIRECTION ( 'NONE',  ( 0.000000000000000000, 0.000000000000000000, 1.000000000000000000 ) ) ;
#3482 = ORIENTED_EDGE ( 'NONE', *, *, #6191, .T. ) ;
#3483 = CIRCLE ( 'NONE', #7884, 4.799999999999999822 ) ;
#3484 = CARTESIAN_POINT ( 'NONE',  ( -15.00000000000000000, 40.00000000000000711, 2.000000000000000000 ) ) ;
#3485 = ORIENTED_EDGE ( 'NONE', *, *, #746, .T. ) ;
#3486 = PRESENTATION_STYLE_ASSIGNMENT (( #10110 ) ) ;
#3487 = VERTEX_POINT ( 'NONE', #372 ) ;
#3488 = DIRECTION ( 'NONE',  ( 1.000000000000000000, 0.000000000000000000, 0.000000000000000000 ) ) ;
#3489 = EDGE_CURVE ( 'NONE', #4720, #4328, #8056, .T. ) ;
#3490 = CYLINDRICAL_SURFACE ( 'NONE', #8177, 27.00000000002699707 ) ;
#3491 = ADVANCED_FACE ( 'NONE', ( #1314 ), #3090, .F. ) ;
#3492 = AXIS2_PLACEMENT_3D ( 'NONE', #11455, #9475, #9526 ) ;
#3493 = EDGE_CURVE ( 'NONE', #8510, #11907, #2645, .T. ) ;
#3494 = VERTEX_POINT ( 'NONE', #4187 ) ;
#3495 = PLANE ( 'NONE',  #2409 ) ;
#3496 = EDGE_LOOP ( 'NONE', ( #4984, #1292, #3729, #1243 ) ) ;
#3497 = DIRECTION ( 'NONE',  ( 0.000000000000000000, 0.000000000000000000, 1.000000000000000000 ) ) ;
#3498 = EDGE_LOOP ( 'NONE', ( #6299, #5712, #9511, #7126 ) ) ;
#3499 = AXIS2_PLACEMENT_3D ( 'NONE', #362, #1307, #2184 ) ;
#3500 = PRESENTATION_STYLE_ASSIGNMENT (( #1180 ) ) ;
#3501 = CARTESIAN_POINT ( 'NONE',  ( 4.999999999999999112, -15.37949036966221072, 13.17168466712922914 ) ) ;
#3502 = VERTEX_POINT ( 'NONE', #10827 ) ;
#3503 = CARTESIAN_POINT ( 'NONE',  ( 0.000000000000000000, 0.000000000000000000, 0.000000000000000000 ) ) ;
#3504 = DIRECTION ( 'NONE',  ( 0.000000000000000000, 0.000000000000000000, -1.000000000000000000 ) ) ;
#3505 = AXIS2_PLACEMENT_3D ( 'NONE', #6750, #1994, #6626 ) ;
#3506 = CARTESIAN_POINT ( 'NONE',  ( -10.00000000000000000, 0.000000000000000000, 0.000000000000000000 ) ) ;
#3507 = CARTESIAN_POINT ( 'NONE',  ( -13.05124837953327344, 12.50000000000000000, -24.50000000000000000 ) ) ;
#3508 = CARTESIAN_POINT ( 'NONE',  ( 20.00000000000000000, 40.00000000000001421, 12.50000000000000000 ) ) ;
#3509 = ORIENTED_EDGE ( 'NONE', *, *, #11430, .T. ) ;
#3510 = VERTEX_POINT ( 'NONE', #2261 ) ;
#3511 = CARTESIAN_POINT ( 'NONE',  ( 4.999999999999999112, 0.000000000000000000, 0.000000000000000000 ) ) ;
#3512 = FACE_OUTER_BOUND ( 'NONE', #11941, .T. ) ;
#3513 = ORIENTED_EDGE ( 'NONE', *, *, #6548, .F. ) ;
#3514 = DIRECTION ( 'NONE',  ( -1.000000000000000000, -1.734723475976807094E-16, 0.000000000000000000 ) ) ;
#3515 = EDGE_CURVE ( 'NONE', #9230, #1528, #1257, .T. ) ;
#3516 = ORIENTED_EDGE ( 'NONE', *, *, #63, .F. ) ;
#3517 = CARTESIAN_POINT ( 'NONE',  ( 0.000000000000000000, -14.41081992069325857, 22.83261415639497827 ) ) ;
#3518 = EDGE_CURVE ( 'NONE', #4612, #4657, #6859, .T. ) ;
#3519 = PRODUCT_DEFINITION_SHAPE ( 'NONE', 'NONE',  #6878 ) ;
#3520 = CARTESIAN_POINT ( 'NONE',  ( 4.999999999999999112, -6.283573709965167176, -19.24938187143303026 ) ) ;
#3521 = LINE ( 'NONE', #4324, #10151 ) ;
#3522 = CARTESIAN_POINT ( 'NONE',  ( 0.000000000000000000, 11.41582255376084909, -8.527191590520953213 ) ) ;
#3523 = CARTESIAN_POINT ( 'NONE',  ( -36.00000000000000000, 0.000000000000000000, 0.000000000000000000 ) ) ;
#3524 = VERTEX_POINT ( 'NONE', #6903 ) ;
#3525 = CARTESIAN_POINT ( 'NONE',  ( 42.00000000000000000, -3.058102613202345665, 3.699730856038719207 ) ) ;
#3526 = DIRECTION ( 'NONE',  ( 0.000000000000000000, 0.000000000000000000, 1.000000000000000000 ) ) ;
#3527 = VERTEX_POINT ( 'NONE', #10704 ) ;
#3528 = CARTESIAN_POINT ( 'NONE',  ( 20.00000000000000000, 44.00000000000002132, 12.50000000000000000 ) ) ;
#3529 = UNCERTAINTY_MEASURE_WITH_UNIT (LENGTH_MEASURE( 1.000000000000000082E-05 ), #3001, 'distance_accuracy_value', 'NONE');
#3530 = ORIENTED_EDGE ( 'NONE', *, *, #5182, .T. ) ;
#3531 = CARTESIAN_POINT ( 'NONE',  ( -20.63749999999999929, 0.000000000000000000, -5.525000000000000355 ) ) ;
#3532 = DIRECTION ( 'NONE',  ( -1.000000000000000000, -3.903127820947815962E-18, 0.000000000000000000 ) ) ;
#3533 = FACE_OUTER_BOUND ( 'NONE', #2059, .T. ) ;
#3534 = CARTESIAN_POINT ( 'NONE',  ( 37.00000000000000711, -3.606021680338235225, -38.83193945118931367 ) ) ;
#3535 = DIRECTION ( 'NONE',  ( 0.000000000000000000, 0.3826834323650905589, -0.9238795325112864054 ) ) ;
#3536 = EDGE_LOOP ( 'NONE', ( #10683, #11862, #1876, #1283 ) ) ;
#3537 = CARTESIAN_POINT ( 'NONE',  ( -10.00000000000000000, 0.000000000000000000, 0.000000000000000000 ) ) ;
#3538 = ORIENTED_EDGE ( 'NONE', *, *, #5874, .T. ) ;
#3539 = CARTESIAN_POINT ( 'NONE',  ( 24.00000000000000000, 0.000000000000000000, -41.99999999999999289 ) ) ;
#3540 = EDGE_CURVE ( 'NONE', #8258, #1032, #6253, .T. ) ;
#3541 = DIRECTION ( 'NONE',  ( 0.000000000000000000, 0.000000000000000000, 1.000000000000000000 ) ) ;
#3542 = ORIENTED_EDGE ( 'NONE', *, *, #5949, .F. ) ;
#3543 = DIRECTION ( 'NONE',  ( 0.000000000000000000, 0.000000000000000000, -1.000000000000000000 ) ) ;
#3544 = PRODUCT_DEFINITION_SHAPE ( 'NONE', 'NONE',  #12359 ) ;
#3545 = DIRECTION ( 'NONE',  ( -1.000000000000000000, 4.770489558936236458E-18, -6.855277276495154548E-34 ) ) ;
#3546 = VERTEX_POINT ( 'NONE', #6953 ) ;
#3547 = CARTESIAN_POINT ( 'NONE',  ( 1.500000000000001332, 0.000000000000000000, 0.000000000000000000 ) ) ;
#3548 = EDGE_CURVE ( 'NONE', #2796, #10027, #11002, .T. ) ;
#3549 = ORIENTED_EDGE ( 'NONE', *, *, #4269, .F. ) ;
#3550 = CARTESIAN_POINT ( 'NONE',  ( 36.00000000000000000, 0.000000000000000000, -44.50000000000000000 ) ) ;
#3551 = VERTEX_POINT ( 'NONE', #12059 ) ;
#3552 = EDGE_CURVE ( 'NONE', #9384, #9485, #622, .T. ) ;
#3553 =( NAMED_UNIT ( * ) SI_UNIT ( $, .STERADIAN. ) SOLID_ANGLE_UNIT ( ) );
#3554 = ADVANCED_FACE ( 'NONE', ( #12171, #552, #7329 ), #689, .F. ) ;
#3555 = DIRECTION ( 'NONE',  ( -1.000000000000000000, -0.000000000000000000, -0.000000000000000000 ) ) ;
#3556 = ORIENTED_EDGE ( 'NONE', *, *, #3390, .F. ) ;
#3557 = CARTESIAN_POINT ( 'NONE',  ( 0.000000000000000000, 0.000000000000000000, 0.000000000000000000 ) ) ;
#3558 = CARTESIAN_POINT ( 'NONE',  ( -13.05124837953327344, -12.50000000000000000, -41.99999999999999289 ) ) ;
#3559 = AXIS2_PLACEMENT_3D ( 'NONE', #2611, #7375, #11914 ) ;
#3560 = VECTOR ( 'NONE', #7965, 1000.000000000000000 ) ;
#3561 = LINE ( 'NONE', #551, #62 ) ;
#3562 = CARTESIAN_POINT ( 'NONE',  ( 4.999999999999999112, 0.000000000000000000, 0.000000000000000000 ) ) ;
#3563 = ORIENTED_EDGE ( 'NONE', *, *, #4057, .F. ) ;
#3564 = ORIENTED_EDGE ( 'NONE', *, *, #10497, .F. ) ;
#3565 = CYLINDRICAL_SURFACE ( 'NONE', #4857, 14.24900000001425227 ) ;
#3566 = EDGE_CURVE ( 'NONE', #11321, #5923, #7048, .T. ) ;
#3567 = CARTESIAN_POINT ( 'NONE',  ( 4.999999999999999112, -14.14998813191268390, -1.676853263448035536 ) ) ;
#3568 = EDGE_CURVE ( 'NONE', #10665, #11306, #11231, .T. ) ;
#3569 = EDGE_CURVE ( 'NONE', #11219, #7247, #4846, .T. ) ;
#3570 = ORIENTED_EDGE ( 'NONE', *, *, #8614, .F. ) ;
#3571 = FACE_BOUND ( 'NONE', #7648, .T. ) ;
#3572 = VERTEX_POINT ( 'NONE', #8196 ) ;
#3573 = CARTESIAN_POINT ( 'NONE',  ( 2.500000000000000000, 1.178949249685213863, -2.042000000000001148 ) ) ;
#3574 = CIRCLE ( 'NONE', #5763, 25.00000000000000000 ) ;
#3575 = CIRCLE ( 'NONE', #9963, 6.500000000000000888 ) ;
#3576 = CARTESIAN_POINT ( 'NONE',  ( 6.080745460913608902, 0.5192545390863916310, -1.000000000000000000 ) ) ;
#3577 = DIRECTION ( 'NONE',  ( -1.000000000000000000, 0.000000000000000000, 0.000000000000000000 ) ) ;
#3578 = EDGE_CURVE ( 'NONE', #8475, #11902, #4653, .T. ) ;
#3579 = ORIENTED_EDGE ( 'NONE', *, *, #645, .T. ) ;
#3580 = ADVANCED_FACE ( 'NONE', ( #10183, #5378 ), #2368, .T. ) ;
#3581 = CARTESIAN_POINT ( 'NONE',  ( 0.000000000000000000, 13.17168466712950092, -15.37949036966198157 ) ) ;
#3582 = DIRECTION ( 'NONE',  ( 1.000000000000000000, 0.000000000000000000, 0.000000000000000000 ) ) ;
#3583 = AXIS2_PLACEMENT_3D ( 'NONE', #1546, #5362, #2926 ) ;
#3584 = ORIENTED_EDGE ( 'NONE', *, *, #1554, .F. ) ;
#3585 = FACE_OUTER_BOUND ( 'NONE', #802, .T. ) ;
#3586 = DIRECTION ( 'NONE',  ( -1.000000000000000000, 0.000000000000000000, 0.000000000000000000 ) ) ;
#3587 = PRESENTATION_LAYER_ASSIGNMENT (  '', '', ( #1993 ) ) ;
#3588 = ORIENTED_EDGE ( 'NONE', *, *, #265, .T. ) ;
#3589 = ORIENTED_EDGE ( 'NONE', *, *, #2958, .F. ) ;
#3590 = CIRCLE ( 'NONE', #2187, 7.399999999999999467 ) ;
#3591 = AXIS2_PLACEMENT_3D ( 'NONE', #1309, #2186, #8011 ) ;
#3592 = CARTESIAN_POINT ( 'NONE',  ( 2.500000000000000000, 0.000000000000000000, 0.000000000000000000 ) ) ;
#3593 = CIRCLE ( 'NONE', #5586, 21.00000000002100009 ) ;
#3594 = CARTESIAN_POINT ( 'NONE',  ( 0.5000000000000000000, -6.429618962271402616, -1.000000000000000000 ) ) ;
#3595 = DIRECTION ( 'NONE',  ( -1.000000000000000000, -0.000000000000000000, -0.000000000000000000 ) ) ;
#3596 = EDGE_CURVE ( 'NONE', #11316, #4059, #11824, .T. ) ;
#3597 = CARTESIAN_POINT ( 'NONE',  ( 0.000000000000000000, -15.37949036966221072, 13.17168466712922914 ) ) ;
#3598 = DIRECTION ( 'NONE',  ( 0.000000000000000000, 0.000000000000000000, -1.000000000000000000 ) ) ;
#3599 = ORIENTED_EDGE ( 'NONE', *, *, #1042, .T. ) ;
#3600 = VERTEX_POINT ( 'NONE', #11919 ) ;
#3601 = CARTESIAN_POINT ( 'NONE',  ( 0.000000000000000000, 5.051668046482832750E-16, -4.000000000000000000 ) ) ;
#3602 = CIRCLE ( 'NONE', #6600, 20.24900000002024569 ) ;
#3603 = VERTEX_POINT ( 'NONE', #9326 ) ;
#3604 = CARTESIAN_POINT ( 'NONE',  ( 36.00000000000000711, 1.456773409934505593E-31, -41.99999999999998579 ) ) ;
#3605 = VERTEX_POINT ( 'NONE', #1558 ) ;
#3606 = VECTOR ( 'NONE', #7815, 1000.000000000000114 ) ;
#3607 = DIRECTION ( 'NONE',  ( 0.000000000000000000, 0.000000000000000000, -1.000000000000000000 ) ) ;
#3608 = CARTESIAN_POINT ( 'NONE',  ( 4.999999999999999112, -26.60936692326693276, 4.576198416197154728 ) ) ;
#3609 = COLOUR_RGB ( '',1.000000000000000000, 0.9490196078431372140, 0.9098039215686274384 ) ;
#3610 = ORIENTED_EDGE ( 'NONE', *, *, #3623, .T. ) ;
#3611 = DIRECTION ( 'NONE',  ( 0.000000000000000000, 0.000000000000000000, 1.000000000000000000 ) ) ;
#3612 = CIRCLE ( 'NONE', #6408, 25.00000000000000000 ) ;
#3613 = ORIENTED_EDGE ( 'NONE', *, *, #4876, .F. ) ;
#3614 = CARTESIAN_POINT ( 'NONE',  ( 29.00000000000000000, 0.000000000000000000, -34.49999999999999289 ) ) ;
#3615 = ORIENTED_EDGE ( 'NONE', *, *, #8530, .F. ) ;
#3616 = AXIS2_PLACEMENT_3D ( 'NONE', #4826, #7766, #4701 ) ;
#3617 = DIRECTION ( 'NONE',  ( 0.000000000000000000, 1.000000000000000000, 3.491481338843133750E-15 ) ) ;
#3618 = AXIS2_PLACEMENT_3D ( 'NONE', #10678, #3798, #5734 ) ;
#3619 = EDGE_LOOP ( 'NONE', ( #7770, #11046, #10941, #7275 ) ) ;
#3620 = DIRECTION ( 'NONE',  ( -1.000000000000000000, -0.000000000000000000, -0.000000000000000000 ) ) ;
#3621 = AXIS2_PLACEMENT_3D ( 'NONE', #2470, #529, #8233 ) ;
#3622 = AXIS2_PLACEMENT_3D ( 'NONE', #6989, #9877, #2989 ) ;
#3623 = EDGE_CURVE ( 'NONE', #1333, #7347, #5853, .T. ) ;
#3624 = DIRECTION ( 'NONE',  ( 0.000000000000000000, -0.7071067811865389130, -0.7071067811865562325 ) ) ;
#3625 = ADVANCED_FACE ( 'NONE', ( #10131 ), #2501, .T. ) ;
#3626 = VECTOR ( 'NONE', #5957, 1000.000000000000000 ) ;
#3627 = AXIS2_PLACEMENT_3D ( 'NONE', #2714, #7482, #660 ) ;
#3628 = CIRCLE ( 'NONE', #8235, 5.999999999999999112 ) ;
#3629 = DIRECTION ( 'NONE',  ( 0.000000000000000000, 0.000000000000000000, 1.000000000000000000 ) ) ;
#3630 = DIRECTION ( 'NONE',  ( 0.000000000000000000, -6.987080667121817133E-15, 1.000000000000000000 ) ) ;
#3631 = ORIENTED_EDGE ( 'NONE', *, *, #9232, .T. ) ;
#3632 = ORIENTED_EDGE ( 'NONE', *, *, #953, .T. ) ;
#3633 = LINE ( 'NONE', #10311, #66 ) ;
#3634 = CYLINDRICAL_SURFACE ( 'NONE', #633, 27.00000000002699707 ) ;
#3635 = CARTESIAN_POINT ( 'NONE',  ( 20.00000000000000000, 0.000000000000000000, 0.000000000000000000 ) ) ;
#3636 = ORIENTED_EDGE ( 'NONE', *, *, #3045, .T. ) ;
#3637 = CARTESIAN_POINT ( 'NONE',  ( 45.00000000000000000, 0.000000000000000000, 0.000000000000000000 ) ) ;
#3638 =( GEOMETRIC_REPRESENTATION_CONTEXT ( 3 ) GLOBAL_UNCERTAINTY_ASSIGNED_CONTEXT ( ( #8529 ) ) GLOBAL_UNIT_ASSIGNED_CONTEXT ( ( #1548, #4494, #3553 ) ) REPRESENTATION_CONTEXT ( 'NONE', 'WORKASPACE' ) );
#3639 = VECTOR ( 'NONE', #11685, 1000.000000000000000 ) ;
#3640 = EDGE_CURVE ( 'NONE', #863, #9490, #8448, .T. ) ;
#3641 = CIRCLE ( 'NONE', #7654, 1.199999999999999956 ) ;
#3642 = EDGE_CURVE ( 'NONE', #9710, #1032, #1448, .T. ) ;
#3643 = EDGE_CURVE ( 'NONE', #7872, #5033, #11632, .T. ) ;
#3644 = EDGE_CURVE ( 'NONE', #9094, #3359, #3449, .T. ) ;
#3645 = DIRECTION ( 'NONE',  ( 0.000000000000000000, 0.000000000000000000, 1.000000000000000000 ) ) ;
#3646 = ORIENTED_EDGE ( 'NONE', *, *, #8677, .F. ) ;
#3647 = ORIENTED_EDGE ( 'NONE', *, *, #3552, .T. ) ;
#3648 = DIRECTION ( 'NONE',  ( 0.000000000000000000, -1.000000000000000000, -1.047444401652940007E-14 ) ) ;
#3649 = PLANE ( 'NONE',  #7440 ) ;
#3650 = CIRCLE ( 'NONE', #10642, 9.600000000009604406 ) ;
#3651 = AXIS2_PLACEMENT_3D ( 'NONE', #9303, #9243, #6537 ) ;
#3652 = ORIENTED_EDGE ( 'NONE', *, *, #9761, .F. ) ;
#3653 = FACE_OUTER_BOUND ( 'NONE', #11171, .T. ) ;
#3654 = VECTOR ( 'NONE', #6508, 1000.000000000000000 ) ;
#3655 = CARTESIAN_POINT ( 'NONE',  ( 4.999999999999999112, -8.872489362018088244, -14.40062958310474883 ) ) ;
#3656 = EDGE_LOOP ( 'NONE', ( #10124, #9210, #8933, #10573 ) ) ;
#3657 = LINE ( 'NONE', #11028, #12251 ) ;
#3658 = UNCERTAINTY_MEASURE_WITH_UNIT (LENGTH_MEASURE( 1.000000000000000082E-05 ), #4312, 'distance_accuracy_value', 'NONE');
#3659 = ORIENTED_EDGE ( 'NONE', *, *, #11079, .F. ) ;
#3660 = EDGE_CURVE ( 'NONE', #8639, #4145, #5055, .T. ) ;
#3661 = PRESENTATION_STYLE_ASSIGNMENT (( #12202 ) ) ;
#3662 = FACE_OUTER_BOUND ( 'NONE', #8499, .T. ) ;
#3663 = DIRECTION ( 'NONE',  ( 0.000000000000000000, 0.000000000000000000, 1.000000000000000000 ) ) ;
#3664 = DIRECTION ( 'NONE',  ( 0.000000000000000000, 0.6600126143355578012, 0.7512545167371323940 ) ) ;
#3665 = DIRECTION ( 'NONE',  ( 1.000000000000000000, 0.000000000000000000, 0.000000000000000000 ) ) ;
#3666 = VERTEX_POINT ( 'NONE', #4366 ) ;
#3667 = ORIENTED_EDGE ( 'NONE', *, *, #1571, .T. ) ;
#3668 = DIRECTION ( 'NONE',  ( 0.000000000000000000, -0.4526840589413320126, 0.8916709834801178625 ) ) ;
#3669 = ORIENTED_EDGE ( 'NONE', *, *, #2945, .F. ) ;
#3670 = CARTESIAN_POINT ( 'NONE',  ( 15.00000000000000355, 46.40000000000001990, 0.000000000000000000 ) ) ;
#3671 = CIRCLE ( 'NONE', #5876, 6.500000000000000888 ) ;
#3672 = VERTEX_POINT ( 'NONE', #7274 ) ;
#3673 = DIRECTION ( 'NONE',  ( -1.000000000000000000, 4.770489558936236458E-18, -6.855277276495154548E-34 ) ) ;
#3674 = EDGE_CURVE ( 'NONE', #733, #4573, #2451, .T. ) ;
#3675 = DIRECTION ( 'NONE',  ( -0.000000000000000000, -1.000000000000000000, -0.000000000000000000 ) ) ;
#3676 = ADVANCED_FACE ( 'NONE', ( #9566 ), #4453, .T. ) ;
#3677 = VERTEX_POINT ( 'NONE', #10556 ) ;
#3678 = CARTESIAN_POINT ( 'NONE',  ( 76.00000000000000000, 46.00000000000001421, -41.99999999999999289 ) ) ;
#3679 = AXIS2_PLACEMENT_3D ( 'NONE', #11767, #3292, #6218 ) ;
#3680 = B_SPLINE_CURVE_WITH_KNOTS ( 'NONE', 3,
 ( #9800, #11663, #400, #6108, #6926, #5154, #10727, #1226 ),
 .UNSPECIFIED., .F., .F.,
 ( 4, 2, 2, 4 ),
 ( 0.006406776852013720304, 0.007252600724735226365, 0.007675512661095979829, 0.008098424597456733293 ),
 .UNSPECIFIED. ) ;
#3681 = CARTESIAN_POINT ( 'NONE',  ( 0.000000000000000000, 0.000000000000000000, 4.000000000000000000 ) ) ;
#3682 = ORIENTED_EDGE ( 'NONE', *, *, #2718, .F. ) ;
#3683 = CARTESIAN_POINT ( 'NONE',  ( 2.500000000000000000, 1.178949249685218525, 2.041999999999999371 ) ) ;
#3684 = ORIENTED_EDGE ( 'NONE', *, *, #6547, .T. ) ;
#3685 = DIRECTION ( 'NONE',  ( 0.000000000000000000, 0.4999999999999948375, 0.8660254037844415942 ) ) ;
#3686 = AXIS2_PLACEMENT_3D ( 'NONE', #5015, #11751, #9721 ) ;
#3687 = ORIENTED_EDGE ( 'NONE', *, *, #5099, .T. ) ;
#3688 = DIRECTION ( 'NONE',  ( -1.000000000000000000, 0.000000000000000000, -0.000000000000000000 ) ) ;
#3689 = CARTESIAN_POINT ( 'NONE',  ( 4.999999999999999112, -15.37949036966202598, -13.17168466712944408 ) ) ;
#3690 = VECTOR ( 'NONE', #10561, 1000.000000000000000 ) ;
#3691 = DIRECTION ( 'NONE',  ( -0.000000000000000000, 1.000000000000000000, 0.000000000000000000 ) ) ;
#3692 = DIRECTION ( 'NONE',  ( -1.000000000000000000, 0.000000000000000000, -0.000000000000000000 ) ) ;
#3693 = ORIENTED_EDGE ( 'NONE', *, *, #886, .F. ) ;
#3694 = VERTEX_POINT ( 'NONE', #932 ) ;
#3695 = DIRECTION ( 'NONE',  ( 1.000000000000000000, 0.000000000000000000, 0.000000000000000000 ) ) ;
#3696 =( LENGTH_UNIT ( ) NAMED_UNIT ( * ) SI_UNIT ( .MILLI., .METRE. ) );
#3697 = FACE_OUTER_BOUND ( 'NONE', #5011, .T. ) ;
#3698 = DIRECTION ( 'NONE',  ( -1.000000000000000000, -0.000000000000000000, -0.000000000000000000 ) ) ;
#3699 = EDGE_CURVE ( 'NONE', #11604, #504, #7641, .T. ) ;
#3700 = VERTEX_POINT ( 'NONE', #873 ) ;
#3701 = CARTESIAN_POINT ( 'NONE',  ( 4.999999999999999112, -22.05152472667140628, 15.57980286237465251 ) ) ;
#3702 = APPLICATION_CONTEXT ( 'automotive_design' ) ;
#3703 = AXIS2_PLACEMENT_3D ( 'NONE', #10492, #1739, #9504 ) ;
#3704 = CARTESIAN_POINT ( 'NONE',  ( 26.00000000000000355, 12.50000000000000000, -37.99671038392666134 ) ) ;
#3705 = CARTESIAN_POINT ( 'NONE',  ( -6.080745460913608902, 0.5192545390863924082, -1.000000000000000000 ) ) ;
#3706 = ORIENTED_EDGE ( 'NONE', *, *, #3826, .T. ) ;
#3707 = DIRECTION ( 'NONE',  ( 1.000000000000000000, 0.000000000000000000, 0.000000000000000000 ) ) ;
#3708 = CARTESIAN_POINT ( 'NONE',  ( 37.00000000000000711, 1.456773409934505593E-31, -41.99999999999998579 ) ) ;
#3709 = ORIENTED_EDGE ( 'NONE', *, *, #8848, .F. ) ;
#3710 = EDGE_CURVE ( 'NONE', #9456, #11316, #3884, .T. ) ;
#3711 = DIRECTION ( 'NONE',  ( 0.000000000000000000, 0.000000000000000000, 1.000000000000000000 ) ) ;
#3712 = LINE ( 'NONE', #7346, #8224 ) ;
#3713 = VERTEX_POINT ( 'NONE', #11364 ) ;
#3714 = LINE ( 'NONE', #8718, #2483 ) ;
#3715 = EDGE_CURVE ( 'NONE', #6891, #11408, #5460, .T. ) ;
#3716 = ORIENTED_EDGE ( 'NONE', *, *, #1076, .F. ) ;
#3717 = EDGE_CURVE ( 'NONE', #238, #3187, #2881, .T. ) ;
#3718 =( NAMED_UNIT ( * ) PLANE_ANGLE_UNIT ( ) SI_UNIT ( $, .RADIAN. ) );
#3719 = DIRECTION ( 'NONE',  ( 0.000000000000000000, 0.000000000000000000, 1.000000000000000000 ) ) ;
#3720 = DIRECTION ( 'NONE',  ( 0.000000000000000000, 0.000000000000000000, 1.000000000000000000 ) ) ;
#3721 = CARTESIAN_POINT ( 'NONE',  ( 0.000000000000000000, 13.85025647830082818, -17.79862902732250163 ) ) ;
#3722 = CARTESIAN_POINT ( 'NONE',  ( 2.499999999999999556, 20.41639017900859443, -4.916402349214656020 ) ) ;
#3723 = EDGE_LOOP ( 'NONE', ( #5285, #5130, #462, #7356 ) ) ;
#3724 = ORIENTED_EDGE ( 'NONE', *, *, #11864, .F. ) ;
#3725 = DIRECTION ( 'NONE',  ( 1.000000000000000000, -0.000000000000000000, -0.000000000000000000 ) ) ;
#3726 = ORIENTED_EDGE ( 'NONE', *, *, #9315, .F. ) ;
#3727 = CARTESIAN_POINT ( 'NONE',  ( -1.500000000000001332, 0.000000000000000000, 0.000000000000000000 ) ) ;
#3728 = PRODUCT_CONTEXT ( 'NONE', #7131, 'mechanical' ) ;
#3729 = ORIENTED_EDGE ( 'NONE', *, *, #12154, .T. ) ;
#3730 = PRODUCT_RELATED_PRODUCT_CATEGORY ( 'part', '', ( #7730 ) ) ;
#3731 = DIRECTION ( 'NONE',  ( -1.000000000000000000, -0.000000000000000000, -0.000000000000000000 ) ) ;
#3732 = CARTESIAN_POINT ( 'NONE',  ( 0.000000000000000000, 1.561154383803221579, 20.18872947935931705 ) ) ;
#3733 = VERTEX_POINT ( 'NONE', #996 ) ;
#3734 = ORIENTED_EDGE ( 'NONE', *, *, #2320, .T. ) ;
#3735 = CARTESIAN_POINT ( 'NONE',  ( 4.999999999999999112, -8.527191590520994069, -11.41582255376081889 ) ) ;
#3736 = FACE_OUTER_BOUND ( 'NONE', #4859, .T. ) ;
#3737 = FACE_OUTER_BOUND ( 'NONE', #11421, .T. ) ;
#3738 = EDGE_LOOP ( 'NONE', ( #6185, #2964, #10408, #5431 ) ) ;
#3739 = EDGE_CURVE ( 'NONE', #4243, #4722, #12025, .T. ) ;
#3740 = ADVANCED_FACE ( 'NONE', ( #5692 ), #3815, .F. ) ;
#3741 = DIRECTION ( 'NONE',  ( 0.000000000000000000, 0.5000000000000009992, -0.8660254037844381525 ) ) ;
#3742 = EDGE_LOOP ( 'NONE', ( #1675, #2009, #1781, #3213 ) ) ;
#3743 = LINE ( 'NONE', #5614, #6713 ) ;
#3744 = ORIENTED_EDGE ( 'NONE', *, *, #3141, .F. ) ;
#3745 = CARTESIAN_POINT ( 'NONE',  ( 50.00005079999999680, 4.769696007084728073, 1.500000000000000000 ) ) ;
#3746 = CYLINDRICAL_SURFACE ( 'NONE', #11380, 9.600000000009599077 ) ;
#3747 = LINE ( 'NONE', #6704, #10345 ) ;
#3748 = CARTESIAN_POINT ( 'NONE',  ( 4.999999999999999112, -5.984728032764810024, -21.74405275335764287 ) ) ;
#3749 = ORIENTED_EDGE ( 'NONE', *, *, #10083, .F. ) ;
#3750 = ORIENTED_EDGE ( 'NONE', *, *, #1673, .F. ) ;
#3751 = LINE ( 'NONE', #6511, #7459 ) ;
#3752 = APPLICATION_PROTOCOL_DEFINITION ( 'draft international standard', 'automotive_design', 1998, #3308 ) ;
#3753 = DIRECTION ( 'NONE',  ( -0.000000000000000000, 1.000000000000000000, 1.224646799147353207E-16 ) ) ;
#3754 = LINE ( 'NONE', #6513, #5293 ) ;
#3755 = ORIENTED_EDGE ( 'NONE', *, *, #7797, .F. ) ;
#3756 = CARTESIAN_POINT ( 'NONE',  ( 5.686050877451574337, -5.768780236673276995, 0.000000000000000000 ) ) ;
#3757 = DIRECTION ( 'NONE',  ( -1.000000000000000000, 0.000000000000000000, 0.000000000000000000 ) ) ;
#3758 = CARTESIAN_POINT ( 'NONE',  ( -4.078421086530219064, -3.990950201428956845, -1.000000000000000000 ) ) ;
#3759 = LINE ( 'NONE', #6656, #7257 ) ;
#3760 = LINE ( 'NONE', #9521, #6439 ) ;
#3761 = VERTEX_POINT ( 'NONE', #1941 ) ;
#3762 = DIRECTION ( 'NONE',  ( 1.000000000000000000, 0.000000000000000000, 0.000000000000000000 ) ) ;
#3763 = DIRECTION ( 'NONE',  ( -1.000000000000000000, 0.000000000000000000, 0.000000000000000000 ) ) ;
#3764 = AXIS2_PLACEMENT_3D ( 'NONE', #10737, #11612, #7061 ) ;
#3765 = VERTEX_POINT ( 'NONE', #11305 ) ;
#3766 = CARTESIAN_POINT ( 'NONE',  ( 4.999999999999999112, -2.791921004064099154, -22.37914155802288363 ) ) ;
#3767 = UNCERTAINTY_MEASURE_WITH_UNIT (LENGTH_MEASURE( 1.000000000000000082E-05 ), #4615, 'distance_accuracy_value', 'NONE');
#3768 = TOROIDAL_SURFACE ( 'NONE', #7166, 6.250000000000000000, 0.7500000000000000000 ) ;
#3769 = ORIENTED_EDGE ( 'NONE', *, *, #1423, .F. ) ;
#3770 = AXIS2_PLACEMENT_3D ( 'NONE', #20, #3846, #7672 ) ;
#3771 = EDGE_CURVE ( 'NONE', #6266, #8991, #3861, .T. ) ;
#3772 = SURFACE_STYLE_USAGE ( .BOTH. , #8534 ) ;
#3773 = AXIS2_PLACEMENT_3D ( 'NONE', #12073, #1524, #3396 ) ;
#3774 = CARTESIAN_POINT ( 'NONE',  ( 0.000000000000000000, 4.576198416197625463, -26.60936692326685815 ) ) ;
#3775 = LINE ( 'NONE', #1849, #5970 ) ;
#3776 = ADVANCED_FACE ( 'NONE', ( #10499 ), #1746, .T. ) ;
#3777 = CARTESIAN_POINT ( 'NONE',  ( 0.000000000000000000, 0.000000000000000000, 0.000000000000000000 ) ) ;
#3778 = DIRECTION ( 'NONE',  ( -1.000000000000000000, -0.000000000000000000, 0.000000000000000000 ) ) ;
#3779 = ORIENTED_EDGE ( 'NONE', *, *, #8048, .T. ) ;
#3780 = ORIENTED_EDGE ( 'NONE', *, *, #2717, .F. ) ;
#3781 = DIRECTION ( 'NONE',  ( 1.000000000000000000, 0.000000000000000000, 0.000000000000000000 ) ) ;
#3782 = ORIENTED_EDGE ( 'NONE', *, *, #10630, .T. ) ;
#3783 = CARTESIAN_POINT ( 'NONE',  ( 4.999999999999997335, 4.769696007084728073, 1.500000000000000000 ) ) ;
#3784 = APPLICATION_PROTOCOL_DEFINITION ( 'draft international standard', 'automotive_design', 1998, #672 ) ;
#3785 = VERTEX_POINT ( 'NONE', #5744 ) ;
#3787 = CARTESIAN_POINT ( 'NONE',  ( 37.00000000000000711, 6.519918414551419517, -39.55446041381592437 ) ) ;
#3786 = AXIS2_PLACEMENT_3D ( 'NONE', #4831, #7470, #10323 ) ;
#3788 = CIRCLE ( 'NONE', #7362, 21.00000000002100009 ) ;
#3789 = LINE ( 'NONE', #5542, #8364 ) ;
#3790 = CIRCLE ( 'NONE', #9187, 5.000000000000000000 ) ;
#3791 = ORIENTED_EDGE ( 'NONE', *, *, #1789, .F. ) ;
#3792 = ORIENTED_EDGE ( 'NONE', *, *, #3395, .T. ) ;
#3793 = LINE ( 'NONE', #5795, #8393 ) ;
#3794 = PLANE ( 'NONE',  #11983 ) ;
#3795 = EDGE_CURVE ( 'NONE', #752, #9690, #4811, .T. ) ;
#3796 = EDGE_CURVE ( 'NONE', #10109, #88, #4880, .T. ) ;
#3797 = CARTESIAN_POINT ( 'NONE',  ( 0.000000000000000000, 0.000000000000000000, 0.000000000000000000 ) ) ;
#3799 = EDGE_CURVE ( 'NONE', #7260, #6891, #7703, .T. ) ;
#3798 = DIRECTION ( 'NONE',  ( -1.000000000000000000, -0.000000000000000000, 0.000000000000000000 ) ) ;
#3800 = ORIENTED_EDGE ( 'NONE', *, *, #7710, .F. ) ;
#3801 = CIRCLE ( 'NONE', #5994, 5.000000000000004441 ) ;
#3802 = CARTESIAN_POINT ( 'NONE',  ( 4.999999999999999112, 1.676853263448085052, -14.14998813191267857 ) ) ;
#3803 = VERTEX_POINT ( 'NONE', #6564 ) ;
#3804 =( LENGTH_UNIT ( ) NAMED_UNIT ( * ) SI_UNIT ( .MILLI., .METRE. ) );
#3805 = ORIENTED_EDGE ( 'NONE', *, *, #12032, .F. ) ;
#3806 = CARTESIAN_POINT ( 'NONE',  ( -1.400000000000001910, 6.123233995736766282E-16, 5.000000000000000000 ) ) ;
#3807 = VERTEX_POINT ( 'NONE', #9382 ) ;
#3808 = CARTESIAN_POINT ( 'NONE',  ( 4.999999999999999112, 14.88411597386740404, -8.035066368449049534 ) ) ;
#3809 = AXIS2_PLACEMENT_3D ( 'NONE', #5659, #5714, #6856 ) ;
#3810 = EDGE_CURVE ( 'NONE', #3510, #2990, #54, .T. ) ;
#3811 = AXIS2_PLACEMENT_3D ( 'NONE', #194, #7899, #7952 ) ;
#3812 = AXIS2_PLACEMENT_3D ( 'NONE', #9363, #10237, #12096 ) ;
#3813 = DIRECTION ( 'NONE',  ( -1.000000000000000000, -0.000000000000000000, -0.000000000000000000 ) ) ;
#3814 = DIRECTION ( 'NONE',  ( -1.000000000000000000, 0.000000000000000000, 0.000000000000000000 ) ) ;
#3815 = CYLINDRICAL_SURFACE ( 'NONE', #8860, 6.750000000000000000 ) ;
#3816 = AXIS2_PLACEMENT_3D ( 'NONE', #3322, #2258, #3086 ) ;
#3817 = ORIENTED_EDGE ( 'NONE', *, *, #6474, .T. ) ;
#3818 = DIRECTION ( 'NONE',  ( 0.000000000000000000, 0.000000000000000000, 1.000000000000000000 ) ) ;
#3819 = FILL_AREA_STYLE_COLOUR ( '', #6637 ) ;
#3820 = VECTOR ( 'NONE', #10280, 1000.000000000000000 ) ;
#3821 = CARTESIAN_POINT ( 'NONE',  ( 4.999999999999999112, 0.000000000000000000, 0.000000000000000000 ) ) ;
#3822 = CIRCLE ( 'NONE', #11185, 0.7500000000000000000 ) ;
#3823 = DIRECTION ( 'NONE',  ( -1.000000000000000000, 0.000000000000000000, -0.000000000000000000 ) ) ;
#3824 = ORIENTED_EDGE ( 'NONE', *, *, #3715, .T. ) ;
#3825 = CARTESIAN_POINT ( 'NONE',  ( 1.399999999999999689, 0.000000000000000000, 0.000000000000000000 ) ) ;
#3826 = EDGE_CURVE ( 'NONE', #629, #5533, #10652, .T. ) ;
#3827 = AXIS2_PLACEMENT_3D ( 'NONE', #4106, #7928, #11714 ) ;
#3828 = CIRCLE ( 'NONE', #10806, 6.500000000000000888 ) ;
#3829 = CIRCLE ( 'NONE', #7638, 27.00000000002699707 ) ;
#3830 = CYLINDRICAL_SURFACE ( 'NONE', #800, 9.600000000009600853 ) ;
#3831 = CARTESIAN_POINT ( 'NONE',  ( 2.399999999999999467, 0.000000000000000000, 0.000000000000000000 ) ) ;
#3832 = DIRECTION ( 'NONE',  ( -1.000000000000000000, -0.000000000000000000, 0.000000000000000000 ) ) ;
#3833 = CARTESIAN_POINT ( 'NONE',  ( 5.200000000000002842, 0.000000000000000000, 0.000000000000000000 ) ) ;
#3834 = VERTEX_POINT ( 'NONE', #2687 ) ;
#3835 = DIRECTION ( 'NONE',  ( 0.000000000000000000, 0.000000000000000000, 1.000000000000000000 ) ) ;
#3836 = CARTESIAN_POINT ( 'NONE',  ( 0.000000000000000000, -0.4834863907626938961, 16.90755573046746107 ) ) ;
#3837 = VECTOR ( 'NONE', #3103, 1000.000000000000000 ) ;
#3838 = ORIENTED_EDGE ( 'NONE', *, *, #5995, .F. ) ;
#3839 = CARTESIAN_POINT ( 'NONE',  ( 4.999999999999999112, -1.561154383803364798, 20.18872947935930640 ) ) ;
#3840 = AXIS2_PLACEMENT_3D ( 'NONE', #3093, #1198, #6906 ) ;
#3841 = AXIS2_PLACEMENT_3D ( 'NONE', #4704, #6657, #1011 ) ;
#3842 = VERTEX_POINT ( 'NONE', #799 ) ;
#3843 = AXIS2_PLACEMENT_3D ( 'NONE', #10452, #5752, #1891 ) ;
#3844 = AXIS2_PLACEMENT_3D ( 'NONE', #11834, #3219, #10093 ) ;
#3845 = DIRECTION ( 'NONE',  ( -1.000000000000000000, 0.000000000000000000, 0.000000000000000000 ) ) ;
#3846 = DIRECTION ( 'NONE',  ( -1.000000000000000000, -0.000000000000000000, -0.000000000000000000 ) ) ;
#3847 = AXIS2_PLACEMENT_3D ( 'NONE', #3748, #7450, #10440 ) ;
#3848 = DIRECTION ( 'NONE',  ( -1.000000000000000000, 0.000000000000000000, 0.000000000000000000 ) ) ;
#3849 = CARTESIAN_POINT ( 'NONE',  ( 0.000000000000000000, 14.14998813191269633, -1.676853263447935394 ) ) ;
#3850 = ORIENTED_EDGE ( 'NONE', *, *, #10825, .T. ) ;
#3851 = ORIENTED_EDGE ( 'NONE', *, *, #9665, .T. ) ;
#3852 = PRESENTATION_STYLE_ASSIGNMENT (( #5032 ) ) ;
#3853 = EDGE_LOOP ( 'NONE', ( #9207, #6677, #12105, #2036 ) ) ;
#3854 = CARTESIAN_POINT ( 'NONE',  ( 4.999999999999999112, 22.05152472667151642, -15.57980286237449619 ) ) ;
#3855 = EDGE_CURVE ( 'NONE', #9683, #6067, #459, .T. ) ;
#3856 = EDGE_LOOP ( 'NONE', ( #674, #10337 ) ) ;
#3857 = AXIS2_PLACEMENT_3D ( 'NONE', #7117, #9066, #7174 ) ;
#3858 = AXIS2_PLACEMENT_3D ( 'NONE', #9769, #10826, #7135 ) ;
#3859 = COLOUR_RGB ( '',0.8941176470588234615, 0.8941176470588234615, 0.8941176470588234615 ) ;
#3860 = EDGE_CURVE ( 'NONE', #2532, #5984, #6942, .T. ) ;
#3861 = CIRCLE ( 'NONE', #8259, 27.00000000002699707 ) ;
#3862 = VERTEX_POINT ( 'NONE', #4933 ) ;
#3863 = ORIENTED_EDGE ( 'NONE', *, *, #11942, .F. ) ;
#3864 = CARTESIAN_POINT ( 'NONE',  ( 5.000000000000004441, 5.204748896376250699E-16, -4.250000000000000000 ) ) ;
#3865 = CARTESIAN_POINT ( 'NONE',  ( 51.00000000000000000, 3.500000000000001332, -45.49999999999998579 ) ) ;
#3866 = DIRECTION ( 'NONE',  ( -1.000000000000000000, 0.000000000000000000, 0.000000000000000000 ) ) ;
#3867 = LINE ( 'NONE', #2980, #7824 ) ;
#3868 = ORIENTED_EDGE ( 'NONE', *, *, #12168, .F. ) ;
#3869 = CIRCLE ( 'NONE', #7870, 5.000000000000000000 ) ;
#3870 = DIRECTION ( 'NONE',  ( -1.000000000000000000, -0.000000000000000000, 0.000000000000000000 ) ) ;
#3871 = VERTEX_POINT ( 'NONE', #2122 ) ;
#3872 = APPLICATION_CONTEXT ( 'automotive_design' ) ;
#3873 = EDGE_CURVE ( 'NONE', #12064, #8607, #355, .T. ) ;
#3874 = SURFACE_SIDE_STYLE ('',( #11299 ) ) ;
#3875 = VERTEX_POINT ( 'NONE', #9883 ) ;
#3876 = CARTESIAN_POINT ( 'NONE',  ( 2.500000000000000000, 1.178949249685218525, 2.041999999999999371 ) ) ;
#3877 = EDGE_CURVE ( 'NONE', #5016, #8451, #7268, .T. ) ;
#3878 = VERTEX_POINT ( 'NONE', #6066 ) ;
#3879 = CARTESIAN_POINT ( 'NONE',  ( 0.000000000000000000, 0.000000000000000000, 0.000000000000000000 ) ) ;
#3880 = ADVANCED_FACE ( 'NONE', ( #307 ), #2176, .F. ) ;
#3881 = MECHANICAL_DESIGN_GEOMETRIC_PRESENTATION_REPRESENTATION (  '', ( #9073 ), #11055 ) ;
#3882 = CARTESIAN_POINT ( 'NONE',  ( -36.00000000000000711, -7.960204194457796463E-16, -6.500000000000000888 ) ) ;
#3883 = DIRECTION ( 'NONE',  ( 1.000000000000000000, 0.000000000000000000, 0.000000000000000000 ) ) ;
#3884 = LINE ( 'NONE', #6643, #3654 ) ;
#3885 = ORIENTED_EDGE ( 'NONE', *, *, #5870, .F. ) ;
#3886 = DIRECTION ( 'NONE',  ( -1.000000000000000000, -0.000000000000000000, -0.000000000000000000 ) ) ;
#3887=STYLED_ITEM('',(#12412),#4645);
#3888 =( LENGTH_UNIT ( ) NAMED_UNIT ( * ) SI_UNIT ( .MILLI., .METRE. ) );
#3889 = CARTESIAN_POINT ( 'NONE',  ( 5.000000000000004441, 0.000000000000000000, 0.000000000000000000 ) ) ;
#3890 = CARTESIAN_POINT ( 'NONE',  ( 50.00005079999999680, 6.799999999999999822, 1.500000000000000000 ) ) ;
#3891 = ORIENTED_EDGE ( 'NONE', *, *, #7693, .T. ) ;
#3892 = DIRECTION ( 'NONE',  ( 0.000000000000000000, 0.000000000000000000, -1.000000000000000000 ) ) ;
#3893 = PRODUCT_RELATED_PRODUCT_CATEGORY ( 'part', '', ( #5718 ) ) ;
#3894 = AXIS2_PLACEMENT_3D ( 'NONE', #2707, #3472, #8160 ) ;
#3895 = FACE_OUTER_BOUND ( 'NONE', #8671, .T. ) ;
#3896 = CARTESIAN_POINT ( 'NONE',  ( 4.999999999999999112, -4.916402349214724410, 20.41639017900857667 ) ) ;
#3897 = CARTESIAN_POINT ( 'NONE',  ( -36.00000000000000000, 40.00000000000000711, -19.99999999999998934 ) ) ;
#3898 = ORIENTED_EDGE ( 'NONE', *, *, #3518, .T. ) ;
#3899 = CYLINDRICAL_SURFACE ( 'NONE', #7582, 5.000000000000000000 ) ;
#3900 = EDGE_CURVE ( 'NONE', #3355, #9986, #3938, .T. ) ;
#3901 = DIRECTION ( 'NONE',  ( 0.000000000000000000, 0.000000000000000000, -1.000000000000000000 ) ) ;
#3902 = EDGE_CURVE ( 'NONE', #7155, #7438, #1871, .T. ) ;
#3903 = ORIENTED_EDGE ( 'NONE', *, *, #5115, .F. ) ;
#3904 = DIRECTION ( 'NONE',  ( -1.000000000000000000, 0.000000000000000000, 0.000000000000000000 ) ) ;
#3905 = UNCERTAINTY_MEASURE_WITH_UNIT (LENGTH_MEASURE( 1.000000000000000082E-05 ), #1917, 'distance_accuracy_value', 'NONE');
#3906 = AXIS2_PLACEMENT_3D ( 'NONE', #10256, #5513, #7281 ) ;
#3907 = VERTEX_POINT ( 'NONE', #6823 ) ;
#3908 = CARTESIAN_POINT ( 'NONE',  ( 36.00000000000000711, -3.277848209564065307, -45.50652407877909411 ) ) ;
#3909 = CARTESIAN_POINT ( 'NONE',  ( 2.500000000000000000, 3.004629197474318851E-15, 2.042000000000000259 ) ) ;
#3910 = CARTESIAN_POINT ( 'NONE',  ( 25.00000000000000000, 6.123233995736766282E-16, -5.000000000000000000 ) ) ;
#3911 = LINE ( 'NONE', #2773, #4430 ) ;
#3912 = ORIENTED_EDGE ( 'NONE', *, *, #2131, .T. ) ;
#3913 = ORIENTED_EDGE ( 'NONE', *, *, #4888, .T. ) ;
#3914 = VERTEX_POINT ( 'NONE', #11546 ) ;
#3915 = DIRECTION ( 'NONE',  ( -1.000000000000000000, -0.000000000000000000, -0.000000000000000000 ) ) ;
#3916 = ITEM_DEFINED_TRANSFORMATION ( 'NONE', 'NONE', #4841,  #6056 ) ;
#3917 = ORIENTED_EDGE ( 'NONE', *, *, #5852, .T. ) ;
#3918 = ORIENTED_EDGE ( 'NONE', *, *, #8027, .F. ) ;
#3919 = ORIENTED_EDGE ( 'NONE', *, *, #5884, .F. ) ;
#3920 = LINE ( 'NONE', #2050, #1786 ) ;
#3921 = FACE_OUTER_BOUND ( 'NONE', #10251, .T. ) ;
#3922 = CARTESIAN_POINT ( 'NONE',  ( 4.999999999999999112, -14.14998813191270877, 1.676853263447836584 ) ) ;
#3923 = FACE_BOUND ( 'NONE', #3241, .T. ) ;
#3924 = EDGE_CURVE ( 'NONE', #3502, #4444, #2066, .T. ) ;
#3925 = ORIENTED_EDGE ( 'NONE', *, *, #10118, .F. ) ;
#3926 = CYLINDRICAL_SURFACE ( 'NONE', #12149, 9.600000000009600853 ) ;
#3927 = ORIENTED_EDGE ( 'NONE', *, *, #6075, .T. ) ;
#3928 = EDGE_LOOP ( 'NONE', ( #2484, #10016, #2347, #12257 ) ) ;
#3929 = DIRECTION ( 'NONE',  ( 0.000000000000000000, 0.000000000000000000, -1.000000000000000000 ) ) ;
#3930 = ORIENTED_EDGE ( 'NONE', *, *, #4118, .F. ) ;
#3931 = FACE_OUTER_BOUND ( 'NONE', #1196, .T. ) ;
#3932 = DIRECTION ( 'NONE',  ( 0.000000000000000000, 0.000000000000000000, 1.000000000000000000 ) ) ;
#3933 = EDGE_CURVE ( 'NONE', #486, #3875, #8457, .T. ) ;
#3934 = APPLICATION_CONTEXT ( 'automotive_design' ) ;
#3935 = EDGE_CURVE ( 'NONE', #6749, #3551, #5063, .T. ) ;
#3936 = ORIENTED_EDGE ( 'NONE', *, *, #8151, .T. ) ;
#3937 = FACE_OUTER_BOUND ( 'NONE', #7296, .T. ) ;
#3938 = LINE ( 'NONE', #1304, #9067 ) ;
#3939 = ADVANCED_FACE ( 'NONE', ( #11621 ), #5889, .T. ) ;
#3940 = EDGE_LOOP ( 'NONE', ( #5628, #9952 ) ) ;
#3941 = CARTESIAN_POINT ( 'NONE',  ( 42.00000000000000000, 1.908195823574506293E-17, -41.99999999999998579 ) ) ;
#3942 = DIRECTION ( 'NONE',  ( 1.000000000000000000, 3.903127820947815962E-18, 0.000000000000000000 ) ) ;
#3943 = DIRECTION ( 'NONE',  ( -1.000000000000000000, 0.000000000000000000, 0.000000000000000000 ) ) ;
#3944 = ORIENTED_EDGE ( 'NONE', *, *, #1947, .T. ) ;
#3945 = DIRECTION ( 'NONE',  ( -1.000000000000000000, -0.000000000000000000, -0.000000000000000000 ) ) ;
#3946 = CARTESIAN_POINT ( 'NONE',  ( 2.499999999999999556, -20.13931372320393010, 5.950465759858794002 ) ) ;
#3947 = EDGE_CURVE ( 'NONE', #6352, #10042, #6890, .T. ) ;
#3948 = EDGE_CURVE ( 'NONE', #11306, #2216, #7669, .T. ) ;
#3949 = CARTESIAN_POINT ( 'NONE',  ( -19.99999999999999645, 0.000000000000000000, 0.000000000000000000 ) ) ;
#3950 = DIRECTION ( 'NONE',  ( 1.000000000000000000, 0.000000000000000000, 0.000000000000000000 ) ) ;
#3951 = ADVANCED_FACE ( 'NONE', ( #10692 ), #1177, .F. ) ;
#3952 = VERTEX_POINT ( 'NONE', #4065 ) ;
#3953 = CARTESIAN_POINT ( 'NONE',  ( 0.000000000000000000, 6.283573709965309284, 19.24938187143298052 ) ) ;
#3954 = CARTESIAN_POINT ( 'NONE',  ( 0.000000000000000000, 5.622796541391748448, -13.09267581720860996 ) ) ;
#3955 = ORIENTED_EDGE ( 'NONE', *, *, #7519, .F. ) ;
#3956 = FACE_OUTER_BOUND ( 'NONE', #11536, .T. ) ;
#3957 = EDGE_LOOP ( 'NONE', ( #1291, #11999, #7681, #3127 ) ) ;
#3958 = ADVANCED_FACE ( 'NONE', ( #12062 ), #10135, .F. ) ;
#3959 = EDGE_CURVE ( 'NONE', #4240, #3193, #4659, .T. ) ;
#3960 = FACE_OUTER_BOUND ( 'NONE', #12326, .T. ) ;
#3961 = CARTESIAN_POINT ( 'NONE',  ( 4.999999999999999112, -6.283573709965167176, -19.24938187143303026 ) ) ;
#3962 = LINE ( 'NONE', #8105, #8230 ) ;
#3963 = CARTESIAN_POINT ( 'NONE',  ( 0.000000000000000000, 5.955107813822504426, 26.33508479058322749 ) ) ;
#3964 = AXIS2_PLACEMENT_3D ( 'NONE', #5168, #6816, #2062 ) ;
#3965 = ORIENTED_EDGE ( 'NONE', *, *, #10059, .F. ) ;
#3966 = CYLINDRICAL_SURFACE ( 'NONE', #1861, 40.00000000000000711 ) ;
#3967 = VECTOR ( 'NONE', #5024, 1000.000000000000000 ) ;
#3968 = VERTEX_POINT ( 'NONE', #6453 ) ;
#3969 = CARTESIAN_POINT ( 'NONE',  ( 36.00000000000000711, -12.50000000000000000, -41.99999999999999289 ) ) ;
#3970 = PRODUCT_CONTEXT ( 'NONE', #7938, 'mechanical' ) ;
#3971 = VERTEX_POINT ( 'NONE', #11071 ) ;
#3972 = AXIS2_PLACEMENT_3D ( 'NONE', #12170, #2686, #3629 ) ;
#3973 = EDGE_CURVE ( 'NONE', #3871, #1657, #8067, .T. ) ;
#3974 = ORIENTED_EDGE ( 'NONE', *, *, #1602, .T. ) ;
#3975 = EDGE_LOOP ( 'NONE', ( #3724, #4175, #4275, #705 ) ) ;
#3976 = DIRECTION ( 'NONE',  ( 0.000000000000000000, -0.3826834323650773473, -0.9238795325112918455 ) ) ;
#3977 = CARTESIAN_POINT ( 'NONE',  ( 0.000000000000000000, -15.37949036966202598, -13.17168466712944408 ) ) ;
#3978 = DIRECTION ( 'NONE',  ( -0.000000000000000000, 1.000000000000000000, 0.000000000000000000 ) ) ;
#3979 = CARTESIAN_POINT ( 'NONE',  ( -36.00000000000000711, 0.000000000000000000, 40.00000000000000711 ) ) ;
#3980 = ORIENTED_EDGE ( 'NONE', *, *, #9518, .T. ) ;
#3981 = DIRECTION ( 'NONE',  ( -1.000000000000000000, -0.000000000000000000, -0.000000000000000000 ) ) ;
#3982 = CIRCLE ( 'NONE', #6796, 2.000000000000000000 ) ;
#3983 = ORIENTED_EDGE ( 'NONE', *, *, #8738, .T. ) ;
#3984 = SURFACE_STYLE_USAGE ( .BOTH. , #6057 ) ;
#3985 = VERTEX_POINT ( 'NONE', #10936 ) ;
#3986 = COLOUR_RGB ( '',0.8941176470588234615, 0.8941176470588234615, 0.8941176470588234615 ) ;
#3987 = FACE_OUTER_BOUND ( 'NONE', #3656, .T. ) ;
#3988 = ORIENTED_EDGE ( 'NONE', *, *, #4809, .T. ) ;
#3989 = DIRECTION ( 'NONE',  ( 0.000000000000000000, 0.3826834323650905589, -0.9238795325112864054 ) ) ;
#3990 = VECTOR ( 'NONE', #2524, 1000.000000000000000 ) ;
#3991 = DIRECTION ( 'NONE',  ( 0.000000000000000000, 0.000000000000000000, 1.000000000000000000 ) ) ;
#3992 = AXIS2_PLACEMENT_3D ( 'NONE', #2614, #1688, #1620 ) ;
#3993 = ORIENTED_EDGE ( 'NONE', *, *, #2183, .F. ) ;
#3994 = CARTESIAN_POINT ( 'NONE',  ( 4.999999999999999112, 21.74405275335766419, -5.984728032764733641 ) ) ;
#3995 = DIRECTION ( 'NONE',  ( 1.000000000000000000, -0.000000000000000000, -0.000000000000000000 ) ) ;
#3996 = ORIENTED_EDGE ( 'NONE', *, *, #8102, .T. ) ;
#3997 = FACE_OUTER_BOUND ( 'NONE', #10581, .T. ) ;
#3998 = CARTESIAN_POINT ( 'NONE',  ( 42.00000000000000000, 6.799999999999998046, 0.000000000000000000 ) ) ;
#3999 = EDGE_CURVE ( 'NONE', #8668, #8041, #5259, .T. ) ;
#4000 = EDGE_LOOP ( 'NONE', ( #10451, #3419, #3377, #9501 ) ) ;
#4001 = DIRECTION ( 'NONE',  ( -1.000000000000000000, -0.000000000000000000, -0.000000000000000000 ) ) ;
#4002 = VECTOR ( 'NONE', #7635, 1000.000000000000000 ) ;
#4003 = EDGE_CURVE ( 'NONE', #2987, #8258, #5060, .T. ) ;
#4004 = CIRCLE ( 'NONE', #6824, 21.00000000002100009 ) ;
#4005 = CARTESIAN_POINT ( 'NONE',  ( 37.00000000000000711, -3.277848209564066195, -45.50652407877909411 ) ) ;
#4006 = CARTESIAN_POINT ( 'NONE',  ( 36.00000000000000711, 0.000000000000000000, 0.000000000000000000 ) ) ;
#4007 = VECTOR ( 'NONE', #79, 1000.000000000000000 ) ;
#4008 = AXIS2_PLACEMENT_3D ( 'NONE', #7874, #7926, #7051 ) ;
#4009 = CARTESIAN_POINT ( 'NONE',  ( 51.00000000000000000, 3.500000000000001332, -38.49999999999998579 ) ) ;
#4010 = DIRECTION ( 'NONE',  ( -0.000000000000000000, 1.000000000000000000, -0.000000000000000000 ) ) ;
#4011 = EDGE_LOOP ( 'NONE', ( #1395, #7718, #510, #9691 ) ) ;
#4012 = DIRECTION ( 'NONE',  ( 0.000000000000000000, 0.000000000000000000, 1.000000000000000000 ) ) ;
#4013 = DIRECTION ( 'NONE',  ( -1.000000000000000000, -0.000000000000000000, -0.000000000000000000 ) ) ;
#4014 = EDGE_LOOP ( 'NONE', ( #4354, #248 ) ) ;
#4015 = CYLINDRICAL_SURFACE ( 'NONE', #11066, 4.799999999999999822 ) ;
#4016 = EDGE_CURVE ( 'NONE', #7902, #10792, #8656, .T. ) ;
#4017 = ORIENTED_EDGE ( 'NONE', *, *, #3336, .T. ) ;
#4018 = CARTESIAN_POINT ( 'NONE',  ( 42.00000000000000000, 0.000000000000000000, -1.500000000000000000 ) ) ;
#4019 = AXIS2_PLACEMENT_3D ( 'NONE', #8497, #7271, #6689 ) ;
#4020 = CIRCLE ( 'NONE', #9015, 7.200000000007203305 ) ;
#4021 = EDGE_CURVE ( 'NONE', #10764, #1320, #2457, .T. ) ;
#4022 = AXIS2_PLACEMENT_3D ( 'NONE', #5295, #8061, #7113 ) ;
#4023 = EDGE_CURVE ( 'NONE', #3510, #4999, #4724, .T. ) ;
#4024 = AXIS2_PLACEMENT_3D ( 'NONE', #2533, #537, #4346 ) ;
#4025 = ADVANCED_FACE ( 'NONE', ( #3452 ), #4311, .T. ) ;
#4026 = DIRECTION ( 'NONE',  ( -1.000000000000000000, 0.000000000000000000, -0.000000000000000000 ) ) ;
#4027 = DIRECTION ( 'NONE',  ( -1.000000000000000000, -0.000000000000000000, -0.000000000000000000 ) ) ;
#4028 = STYLED_ITEM ( 'NONE', ( #4507 ), #9458 ) ;
#4029 = DIRECTION ( 'NONE',  ( 0.000000000000000000, 1.000000000000000000, -1.224646799147353207E-16 ) ) ;
#4030 = DIRECTION ( 'NONE',  ( 0.000000000000000000, 0.4999999999999950040, 0.8660254037844414832 ) ) ;
#4031 = VECTOR ( 'NONE', #4905, 1000.000000000000000 ) ;
#4032 = CIRCLE ( 'NONE', #9832, 25.00000000000000000 ) ;
#4033 = VERTEX_POINT ( 'NONE', #2555 ) ;
#4034 = AXIS2_PLACEMENT_3D ( 'NONE', #11095, #5349, #9241 ) ;
#4035 = DIRECTION ( 'NONE',  ( 0.000000000000000000, 0.000000000000000000, 1.000000000000000000 ) ) ;
#4036 = VECTOR ( 'NONE', #9333, 1000.000000000000000 ) ;
#4037 = ORIENTED_EDGE ( 'NONE', *, *, #2548, .F. ) ;
#4038 = CARTESIAN_POINT ( 'NONE',  ( 25.00000000000000000, 0.000000000000000000, 0.000000000000000000 ) ) ;
#4039 = CONTEXT_DEPENDENT_SHAPE_REPRESENTATION ( #2414, #10716 ) ;
#4040 = VERTEX_POINT ( 'NONE', #11996 ) ;
#4041 = AXIS2_PLACEMENT_3D ( 'NONE', #937, #6758, #4883 ) ;
#4042 = VECTOR ( 'NONE', #754, 1000.000000000000000 ) ;
#4043 = CYLINDRICAL_SURFACE ( 'NONE', #1187, 9.600000000009600853 ) ;
#4044 = ORIENTED_EDGE ( 'NONE', *, *, #775, .T. ) ;
#4045 = CYLINDRICAL_SURFACE ( 'NONE', #1001, 9.600000000009600853 ) ;
#4046 = DIRECTION ( 'NONE',  ( 0.000000000000000000, 0.000000000000000000, 1.000000000000000000 ) ) ;
#4047 = DIRECTION ( 'NONE',  ( 0.000000000000000000, -0.5000000000000011102, -0.8660254037844379305 ) ) ;
#4048 = CARTESIAN_POINT ( 'NONE',  ( 4.999999999999999112, -8.035066368449308882, 14.88411597386726193 ) ) ;
#4049 = VERTEX_POINT ( 'NONE', #5325 ) ;
#4050 = AXIS2_PLACEMENT_3D ( 'NONE', #592, #478, #4288 ) ;
#4051 = VECTOR ( 'NONE', #5279, 1000.000000000000000 ) ;
#4052 = ORIENTED_EDGE ( 'NONE', *, *, #9260, .F. ) ;
#4053 = CIRCLE ( 'NONE', #6855, 7.200000000007203305 ) ;
#4054 =( NAMED_UNIT ( * ) PLANE_ANGLE_UNIT ( ) SI_UNIT ( $, .RADIAN. ) );
#4055 = EDGE_CURVE ( 'NONE', #9928, #8910, #12229, .T. ) ;
#4057 = EDGE_CURVE ( 'NONE', #2623, #7499, #3869, .T. ) ;
#4056 = VERTEX_POINT ( 'NONE', #9202 ) ;
#4058 = DIRECTION ( 'NONE',  ( 0.000000000000000000, 0.000000000000000000, 1.000000000000000000 ) ) ;
#4059 = VERTEX_POINT ( 'NONE', #692 ) ;
#4060 = CARTESIAN_POINT ( 'NONE',  ( 0.000000000000000000, 46.00000000000001421, -46.00000000000000000 ) ) ;
#4061 = CARTESIAN_POINT ( 'NONE',  ( 4.999999999999999112, 4.916402349214584078, 20.41639017900861219 ) ) ;
#4062 = AXIS2_PLACEMENT_3D ( 'NONE', #3133, #10803, #10742 ) ;
#4063 = ORIENTED_EDGE ( 'NONE', *, *, #968, .F. ) ;
#4064 = CARTESIAN_POINT ( 'NONE',  ( 0.000000000000000000, 14.46592441914965121, 15.22291137398927141 ) ) ;
#4065 = CARTESIAN_POINT ( 'NONE',  ( -0.1920286436967154065, 8.541911424052788811E-16, -6.975000000000000533 ) ) ;
#4066 = ORIENTED_EDGE ( 'NONE', *, *, #6164, .F. ) ;
#4067 = CARTESIAN_POINT ( 'NONE',  ( -1.400000000000000133, 0.000000000000000000, -5.100000000000000533 ) ) ;
#4068 = DIRECTION ( 'NONE',  ( -1.000000000000000000, -0.000000000000000000, -0.000000000000000000 ) ) ;
#4069 = LINE ( 'NONE', #8947, #7300 ) ;
#4070 = VECTOR ( 'NONE', #774, 1000.000000000000000 ) ;
#4071 = EDGE_LOOP ( 'NONE', ( #3980, #9462, #7743, #9623 ) ) ;
#4072 = FACE_OUTER_BOUND ( 'NONE', #10061, .T. ) ;
#4073 = DIRECTION ( 'NONE',  ( 0.000000000000000000, 0.000000000000000000, 1.000000000000000000 ) ) ;
#4074 = CYLINDRICAL_SURFACE ( 'NONE', #11183, 2.500000000000002220 ) ;
#4075 = VECTOR ( 'NONE', #8602, 1000.000000000000000 ) ;
#4076 = DIRECTION ( 'NONE',  ( 1.000000000000000000, 0.000000000000000000, 0.000000000000000000 ) ) ;
#4077 = CARTESIAN_POINT ( 'NONE',  ( 4.999999999999999112, 0.4834863907625768231, 16.90755573046746463 ) ) ;
#4078 = ORIENTED_EDGE ( 'NONE', *, *, #5482, .T. ) ;
#4079 = ADVANCED_FACE ( 'NONE', ( #4506 ), #3565, .T. ) ;
#4080 = DIRECTION ( 'NONE',  ( -1.000000000000000000, 0.000000000000000000, 0.000000000000000000 ) ) ;
#4081 = DIRECTION ( 'NONE',  ( -1.000000000000000000, -0.000000000000000000, -0.000000000000000000 ) ) ;
#4082 = VERTEX_POINT ( 'NONE', #8096 ) ;
#4083 = DIRECTION ( 'NONE',  ( -1.000000000000000000, -0.000000000000000000, -0.000000000000000000 ) ) ;
#4084 = VERTEX_POINT ( 'NONE', #5193 ) ;
#4085 = DIRECTION ( 'NONE',  ( -1.000000000000000000, 0.000000000000000000, -0.000000000000000000 ) ) ;
#4086 = DIRECTION ( 'NONE',  ( -1.000000000000000000, 0.000000000000000000, 0.000000000000000000 ) ) ;
#4087 = LINE ( 'NONE', #1325, #3365 ) ;
#4088 = EDGE_CURVE ( 'NONE', #6055, #4490, #8265, .T. ) ;
#4089 = DIRECTION ( 'NONE',  ( -0.000000000000000000, 1.000000000000000000, -0.000000000000000000 ) ) ;
#4090 = LINE ( 'NONE', #9042, #9251 ) ;
#4091 = ORIENTED_EDGE ( 'NONE', *, *, #6328, .F. ) ;
#4092 = EDGE_CURVE ( 'NONE', #9430, #6597, #11238, .T. ) ;
#4093 = AXIS2_PLACEMENT_3D ( 'NONE', #3635, #6273, #1514 ) ;
#4094 = CARTESIAN_POINT ( 'NONE',  ( -36.00000000000000711, 0.000000000000000000, 0.000000000000000000 ) ) ;
#4095 = EDGE_CURVE ( 'NONE', #1217, #2572, #4458, .T. ) ;
#4096 = VERTEX_POINT ( 'NONE', #5629 ) ;
#4097 = CARTESIAN_POINT ( 'NONE',  ( 2.500000000000000000, -1.178949249685213863, 2.042000000000002924 ) ) ;
#4098 = CONTEXT_DEPENDENT_SHAPE_REPRESENTATION ( #5773, #3544 ) ;
#4099 = VERTEX_POINT ( 'NONE', #12242 ) ;
#4100 = APPLICATION_CONTEXT ( 'automotive_design' ) ;
#4101 = AXIS2_PLACEMENT_3D ( 'NONE', #609, #12101, #7373 ) ;
#4102 = DIRECTION ( 'NONE',  ( 1.000000000000000000, 0.000000000000000000, 0.000000000000000000 ) ) ;
#4103 = EDGE_LOOP ( 'NONE', ( #6208, #2270, #1481 ) ) ;
#4104 = FACE_OUTER_BOUND ( 'NONE', #3291, .T. ) ;
#4105 = DIRECTION ( 'NONE',  ( -1.000000000000000000, 0.000000000000000000, -0.000000000000000000 ) ) ;
#4106 = CARTESIAN_POINT ( 'NONE',  ( 51.00000000000000000, -3.499999999999998668, -38.49999999999998579 ) ) ;
#4107 = CARTESIAN_POINT ( 'NONE',  ( 4.999999999999999112, -5.622796541391473113, -13.09267581720872720 ) ) ;
#4108 = EDGE_LOOP ( 'NONE', ( #3094, #11544, #10303, #1151 ) ) ;
#4109 = EDGE_CURVE ( 'NONE', #8590, #9383, #3751, .T. ) ;
#4110 = EDGE_CURVE ( 'NONE', #718, #5264, #5657, .T. ) ;
#4111 = ORIENTED_EDGE ( 'NONE', *, *, #9518, .F. ) ;
#4112 = FILL_AREA_STYLE_COLOUR ( '', #9845 ) ;
#4113 = EDGE_LOOP ( 'NONE', ( #3996, #10939 ) ) ;
#4114 = CARTESIAN_POINT ( 'NONE',  ( 2.000000000000000000, -6.429618962271402616, -1.000000000000000000 ) ) ;
#4115 = DIRECTION ( 'NONE',  ( -1.000000000000000000, 0.000000000000000000, 0.000000000000000000 ) ) ;
#4116 = DIRECTION ( 'NONE',  ( -1.000000000000000000, 0.000000000000000000, 0.000000000000000000 ) ) ;
#4117 = EDGE_CURVE ( 'NONE', #7407, #1927, #6063, .T. ) ;
#4118 = EDGE_CURVE ( 'NONE', #4159, #6497, #5464, .T. ) ;
#4119 = VERTEX_POINT ( 'NONE', #7643 ) ;
#4120 = CARTESIAN_POINT ( 'NONE',  ( 2.499999999999999556, -20.13931372320384128, -5.950465759859079995 ) ) ;
#4121 = DIRECTION ( 'NONE',  ( 0.000000000000000000, 0.000000000000000000, 1.000000000000000000 ) ) ;
#4122 = VERTEX_POINT ( 'NONE', #4562 ) ;
#4123 = DIRECTION ( 'NONE',  ( 0.000000000000000000, 0.000000000000000000, -1.000000000000000000 ) ) ;
#4124 = CARTESIAN_POINT ( 'NONE',  ( 36.00000000000000000, 0.000000000000000000, -41.99999999999999289 ) ) ;
#4125 = DIRECTION ( 'NONE',  ( -1.000000000000000000, 0.000000000000000000, 0.000000000000000000 ) ) ;
#4126 = ORIENTED_EDGE ( 'NONE', *, *, #7763, .T. ) ;
#4127 = LINE ( 'NONE', #4181, #7391 ) ;
#4128 = DIRECTION ( 'NONE',  ( -1.000000000000000000, 0.000000000000000000, 0.000000000000000000 ) ) ;
#4129 = DIRECTION ( 'NONE',  ( -0.000000000000000000, 1.000000000000000000, 0.000000000000000000 ) ) ;
#4130 = CARTESIAN_POINT ( 'NONE',  ( 51.00000000000000000, -3.499999999999998668, -45.49999999999998579 ) ) ;
#4131 = CARTESIAN_POINT ( 'NONE',  ( 4.999999999999999112, 19.60720892790252989, -11.14352537685181588 ) ) ;
#4132 = DIRECTION ( 'NONE',  ( -1.000000000000000000, -0.000000000000000000, -0.000000000000000000 ) ) ;
#4133 = ORIENTED_EDGE ( 'NONE', *, *, #6071, .T. ) ;
#4134 = ORIENTED_EDGE ( 'NONE', *, *, #2537, .T. ) ;
#4135 = LINE ( 'NONE', #7903, #2579 ) ;
#4136 = DIRECTION ( 'NONE',  ( 0.000000000000000000, 0.000000000000000000, 1.000000000000000000 ) ) ;
#4137 = ORIENTED_EDGE ( 'NONE', *, *, #3317, .T. ) ;
#4138 = CARTESIAN_POINT ( 'NONE',  ( 33.00000000000000000, 0.000000000000000000, -41.99999999999999289 ) ) ;
#4139 = ORIENTED_EDGE ( 'NONE', *, *, #6716, .T. ) ;
#4140 = FACE_OUTER_BOUND ( 'NONE', #8271, .T. ) ;
#4141 = DIRECTION ( 'NONE',  ( -1.000000000000000000, 0.000000000000000000, 0.000000000000000000 ) ) ;
#4142 = DIRECTION ( 'NONE',  ( 1.000000000000000000, 0.000000000000000000, 0.000000000000000000 ) ) ;
#4143 = CARTESIAN_POINT ( 'NONE',  ( 4.999999999999999112, 0.000000000000000000, 0.000000000000000000 ) ) ;
#4144 = ORIENTED_EDGE ( 'NONE', *, *, #4347, .T. ) ;
#4145 = VERTEX_POINT ( 'NONE', #1693 ) ;
#4146 = DIRECTION ( 'NONE',  ( -1.000000000000000000, 4.770489558936235687E-18, -6.855277276495154548E-34 ) ) ;
#4147 = VERTEX_POINT ( 'NONE', #4636 ) ;
#4148 = EDGE_CURVE ( 'NONE', #536, #486, #2265, .T. ) ;
#4149 = EDGE_CURVE ( 'NONE', #5665, #702, #3633, .T. ) ;
#4150 = EDGE_LOOP ( 'NONE', ( #11581, #6039, #1111, #2708 ) ) ;
#4151 = CIRCLE ( 'NONE', #11761, 3.873645755336797780 ) ;
#4152 = CARTESIAN_POINT ( 'NONE',  ( 25.00000000000000000, 0.000000000000000000, 0.000000000000000000 ) ) ;
#4153 = DIRECTION ( 'NONE',  ( 0.000000000000000000, 0.000000000000000000, -1.000000000000000000 ) ) ;
#4154 = CIRCLE ( 'NONE', #1360, 21.00000000002100009 ) ;
#4155 = CARTESIAN_POINT ( 'NONE',  ( 36.00000000000000711, 0.000000000000000000, 0.000000000000000000 ) ) ;
#4156 = FACE_OUTER_BOUND ( 'NONE', #8799, .T. ) ;
#4157 = ORIENTED_EDGE ( 'NONE', *, *, #4302, .T. ) ;
#4158 = DIRECTION ( 'NONE',  ( 0.000000000000000000, 0.8772744497699203059, 0.4799891038147465760 ) ) ;
#4159 = VERTEX_POINT ( 'NONE', #5695 ) ;
#4160 = ORIENTED_EDGE ( 'NONE', *, *, #12157, .T. ) ;
#4162 = DIRECTION ( 'NONE',  ( -1.000000000000000000, -3.903127820947815962E-18, 0.000000000000000000 ) ) ;
#4161 = CIRCLE ( 'NONE', #970, 9.600000000009602630 ) ;
#4163 = AXIS2_PLACEMENT_3D ( 'NONE', #306, #246, #3076 ) ;
#4164 = EDGE_CURVE ( 'NONE', #10334, #9490, #11252, .T. ) ;
#4165 = FACE_OUTER_BOUND ( 'NONE', #829, .T. ) ;
#4166 = EDGE_CURVE ( 'NONE', #3193, #88, #1660, .T. ) ;
#4167 = EDGE_CURVE ( 'NONE', #8321, #12146, #4749, .T. ) ;
#4168 = EDGE_CURVE ( 'NONE', #9094, #8024, #1274, .T. ) ;
#4169 = DIRECTION ( 'NONE',  ( -1.000000000000000000, -0.000000000000000000, -0.000000000000000000 ) ) ;
#4170 = AXIS2_PLACEMENT_3D ( 'NONE', #2672, #1728, #11338 ) ;
#4171 = ORIENTED_EDGE ( 'NONE', *, *, #10444, .F. ) ;
#4172 = CLOSED_SHELL ( 'NONE', ( #5078, #11502, #5002, #8330, #5958, #4295, #7700, #10074, #6499, #11433, #1353, #8462, #10468, #5865, #219, #2788, #11453, #10216, #9282, #8997, #3274, #1880, #5871, #1191, #840, #5612, #1458 ) ) ;
#4173 = DIRECTION ( 'NONE',  ( 0.000000000000000000, 0.000000000000000000, 1.000000000000000000 ) ) ;
#4174 = DIRECTION ( 'NONE',  ( 1.000000000000000000, 0.000000000000000000, 0.000000000000000000 ) ) ;
#4175 = ORIENTED_EDGE ( 'NONE', *, *, #10509, .T. ) ;
#4176 = DIRECTION ( 'NONE',  ( -1.000000000000000000, -3.903127820947815962E-18, 0.000000000000000000 ) ) ;
#4177 = FACE_OUTER_BOUND ( 'NONE', #1560, .T. ) ;
#4178 = FACE_OUTER_BOUND ( 'NONE', #11138, .T. ) ;
#4179 = EDGE_CURVE ( 'NONE', #11838, #4672, #6680, .T. ) ;
#4180 = ORIENTED_EDGE ( 'NONE', *, *, #9449, .F. ) ;
#4181 = CARTESIAN_POINT ( 'NONE',  ( 51.00000000000000000, -3.499999999999998668, -45.49999999999998579 ) ) ;
#4182 = AXIS2_PLACEMENT_3D ( 'NONE', #8957, #2084, #375 ) ;
#4183 = VECTOR ( 'NONE', #12167, 1000.000000000000000 ) ;
#4184 = CARTESIAN_POINT ( 'NONE',  ( 33.00000000000000000, 0.000000000000000000, -49.49999999999999289 ) ) ;
#4185 = CARTESIAN_POINT ( 'NONE',  ( -36.00000000000000711, 34.64101615137755630, 20.00000000000001066 ) ) ;
#4186 = DIRECTION ( 'NONE',  ( 1.000000000000000000, 0.000000000000000000, 0.000000000000000000 ) ) ;
#4187 = CARTESIAN_POINT ( 'NONE',  ( 2.595115354961440524, -7.673029147243177306, -1.000000000000000000 ) ) ;
#4188 = ORIENTED_EDGE ( 'NONE', *, *, #3717, .T. ) ;
#4189 = ORIENTED_EDGE ( 'NONE', *, *, #3411, .T. ) ;
#4190 = CARTESIAN_POINT ( 'NONE',  ( 4.999999999999999112, 0.000000000000000000, 0.000000000000000000 ) ) ;
#4191 = LINE ( 'NONE', #10887, #37 ) ;
#4192 = CIRCLE ( 'NONE', #10789, 7.200000000007202416 ) ;
#4193 = VERTEX_POINT ( 'NONE', #1943 ) ;
#4194 = DIRECTION ( 'NONE',  ( -1.000000000000000000, 0.000000000000000000, 0.000000000000000000 ) ) ;
#4195 = EDGE_CURVE ( 'NONE', #4264, #1798, #70, .T. ) ;
#4196 = EDGE_LOOP ( 'NONE', ( #8551, #786, #8226, #10022 ) ) ;
#4197 = CARTESIAN_POINT ( 'NONE',  ( -10.00000000000000000, 0.000000000000000000, 0.000000000000000000 ) ) ;
#4198 = AXIS2_PLACEMENT_3D ( 'NONE', #12320, #11459, #11393 ) ;
#4199 = AXIS2_PLACEMENT_3D ( 'NONE', #11870, #9086, #5607 ) ;
#4200 = CIRCLE ( 'NONE', #10797, 25.00000000000000000 ) ;
#4201 = DIRECTION ( 'NONE',  ( -1.000000000000000000, -0.000000000000000000, -0.000000000000000000 ) ) ;
#4202 = DIRECTION ( 'NONE',  ( -1.000000000000000000, 0.000000000000000000, 0.000000000000000000 ) ) ;
#4203 = LINE ( 'NONE', #1468, #2838 ) ;
#4204 = ORIENTED_EDGE ( 'NONE', *, *, #2272, .F. ) ;
#4205 = DIRECTION ( 'NONE',  ( 0.000000000000000000, 0.000000000000000000, -1.000000000000000000 ) ) ;
#4206 = ORIENTED_EDGE ( 'NONE', *, *, #9478, .T. ) ;
#4207 = FACE_OUTER_BOUND ( 'NONE', #9244, .T. ) ;
#4208 = CIRCLE ( 'NONE', #7029, 5.100000000000000533 ) ;
#4209 = ADVANCED_BREP_SHAPE_REPRESENTATION ( '', ( #313, #6056 ), #6251 ) ;
#4210 = AXIS2_PLACEMENT_3D ( 'NONE', #11476, #2053, #2924 ) ;
#4211 = EDGE_LOOP ( 'NONE', ( #7282, #5737, #10480, #8162 ) ) ;
#4212 = AXIS2_PLACEMENT_3D ( 'NONE', #7236, #4470, #3663 ) ;
#4213 = AXIS2_PLACEMENT_3D ( 'NONE', #8428, #1674, #724 ) ;
#4214 = CYLINDRICAL_SURFACE ( 'NONE', #7587, 2.700000000000000178 ) ;
#4215 = PRESENTATION_LAYER_ASSIGNMENT (  '', '', ( #4821 ) ) ;
#4216 = AXIS2_PLACEMENT_3D ( 'NONE', #6617, #2675, #6262 ) ;
#4217 = CARTESIAN_POINT ( 'NONE',  ( 0.1481481481481481122, -4.797713218419819903, -1.000000000000000000 ) ) ;
#4218 = DIRECTION ( 'NONE',  ( 0.000000000000000000, 0.000000000000000000, 1.000000000000000000 ) ) ;
#4219 = VECTOR ( 'NONE', #8044, 1000.000000000000000 ) ;
#4220 = AXIS2_PLACEMENT_3D ( 'NONE', #1203, #6961, #8911 ) ;
#4221 = CARTESIAN_POINT ( 'NONE',  ( 4.999999999999997335, 6.123233995736766282E-16, -5.000000000000000000 ) ) ;
#4222 = DIRECTION ( 'NONE',  ( 1.000000000000000000, 0.000000000000000000, 0.000000000000000000 ) ) ;
#4223 = EDGE_CURVE ( 'NONE', #1161, #6545, #1814, .T. ) ;
#4224 = ORIENTED_EDGE ( 'NONE', *, *, #7009, .F. ) ;
#4225 = LINE ( 'NONE', #6235, #8055 ) ;
#4226 = ORIENTED_EDGE ( 'NONE', *, *, #5142, .T. ) ;
#4227 = EDGE_CURVE ( 'NONE', #8435, #5416, #9385, .T. ) ;
#4228 = ORIENTED_EDGE ( 'NONE', *, *, #2653, .F. ) ;
#4229 = AXIS2_PLACEMENT_3D ( 'NONE', #3235, #2289, #5157 ) ;
#4230 = DIRECTION ( 'NONE',  ( 1.000000000000000000, 0.000000000000000000, 0.000000000000000000 ) ) ;
#4231 = AXIS2_PLACEMENT_3D ( 'NONE', #4564, #7455, #2691 ) ;
#4232 = PRODUCT_DEFINITION_SHAPE ( 'NONE', 'NONE',  #12354 ) ;
#4233 = VECTOR ( 'NONE', #11938, 1000.000000000000000 ) ;
#4234 = DIRECTION ( 'NONE',  ( 1.000000000000000000, 0.000000000000000000, 0.000000000000000000 ) ) ;
#4235 = DIRECTION ( 'NONE',  ( 1.000000000000000000, 0.000000000000000000, 0.000000000000000000 ) ) ;
#4236 = PRODUCT_DEFINITION_FORMATION_WITH_SPECIFIED_SOURCE ( 'ANY', '', #6516, .NOT_KNOWN. ) ;
#4237 = AXIS2_PLACEMENT_3D ( 'NONE', #8214, #6579, #11136 ) ;
#4238 = AXIS2_PLACEMENT_3D ( 'NONE', #4124, #427, #8078 ) ;
#4239 = EDGE_CURVE ( 'NONE', #9505, #7260, #10372, .T. ) ;
#4240 = VERTEX_POINT ( 'NONE', #6708 ) ;
#4241 = AXIS2_PLACEMENT_3D ( 'NONE', #7199, #10079, #9140 ) ;
#4242 = CARTESIAN_POINT ( 'NONE',  ( 2.499999999999998668, -5.950465759858725612, -20.13931372320394786 ) ) ;
#4243 = VERTEX_POINT ( 'NONE', #4813 ) ;
#4244 = EDGE_CURVE ( 'NONE', #3280, #8750, #8274, .T. ) ;
#4245 = FACE_OUTER_BOUND ( 'NONE', #12301, .T. ) ;
#4246 = EDGE_CURVE ( 'NONE', #4605, #3761, #3671, .T. ) ;
#4247 = CARTESIAN_POINT ( 'NONE',  ( 4.999999999999999112, 2.791921004064568113, -22.37914155802282323 ) ) ;
#4248 = ORIENTED_EDGE ( 'NONE', *, *, #352, .T. ) ;
#4249 = PLANE ( 'NONE',  #6188 ) ;
#4250 = AXIS2_PLACEMENT_3D ( 'NONE', #5266, #8143, #10253 ) ;
#4251 = CARTESIAN_POINT ( 'NONE',  ( 4.999999999999999112, -14.14998813191268390, -1.676853263448035536 ) ) ;
#4252 = DIRECTION ( 'NONE',  ( -1.000000000000000000, 4.770489558936235687E-18, -6.855277276495154548E-34 ) ) ;
#4253 = CYLINDRICAL_SURFACE ( 'NONE', #9408, 1.999999999999998224 ) ;
#4254 = CARTESIAN_POINT ( 'NONE',  ( 26.00000000000000355, 1.456773409934505593E-31, -41.99999999999998579 ) ) ;
#4255 = CARTESIAN_POINT ( 'NONE',  ( 50.00005079999999680, 4.769696007084728073, 1.500000000000000000 ) ) ;
#4256 = VERTEX_POINT ( 'NONE', #10635 ) ;
#4257 = ORIENTED_EDGE ( 'NONE', *, *, #408, .T. ) ;
#4258 = DIRECTION ( 'NONE',  ( 0.000000000000000000, 0.000000000000000000, -1.000000000000000000 ) ) ;
#4259 = AXIS2_PLACEMENT_3D ( 'NONE', #3259, #2004, #10694 ) ;
#4260 = DIRECTION ( 'NONE',  ( -1.000000000000000000, 0.000000000000000000, 0.000000000000000000 ) ) ;
#4261 = ORIENTED_EDGE ( 'NONE', *, *, #7009, .T. ) ;
#4262 = DIRECTION ( 'NONE',  ( 0.000000000000000000, 0.7900737791495477946, 0.6130117645692876316 ) ) ;
#4263 = PRODUCT_DEFINITION_CONTEXT ( 'detailed design', #3227, 'design' ) ;
#4264 = VERTEX_POINT ( 'NONE', #2072 ) ;
#4265 = CARTESIAN_POINT ( 'NONE',  ( 4.999999999999999112, 0.000000000000000000, 0.000000000000000000 ) ) ;
#4266 = AXIS2_PLACEMENT_3D ( 'NONE', #4038, #393, #2280 ) ;
#4267 =( NAMED_UNIT ( * ) SI_UNIT ( $, .STERADIAN. ) SOLID_ANGLE_UNIT ( ) );
#4268 = CARTESIAN_POINT ( 'NONE',  ( 4.999999999999999112, -14.46592441914954286, -15.22291137398937089 ) ) ;
#4269 = EDGE_CURVE ( 'NONE', #11016, #8473, #5819, .T. ) ;
#4270 = EDGE_CURVE ( 'NONE', #9277, #7555, #5943, .T. ) ;
#4271 = LINE ( 'NONE', #9860, #8444 ) ;
#4272 = DIRECTION ( 'NONE',  ( -1.000000000000000000, -0.000000000000000000, -0.000000000000000000 ) ) ;
#4273 = VERTEX_POINT ( 'NONE', #10744 ) ;
#4274 = DIRECTION ( 'NONE',  ( 0.000000000000000000, 0.000000000000000000, -1.000000000000000000 ) ) ;
#4275 = ORIENTED_EDGE ( 'NONE', *, *, #11678, .T. ) ;
#4276 = CARTESIAN_POINT ( 'NONE',  ( -33.00000000000000000, 0.000000000000000000, -7.500000000000000888 ) ) ;
#4277 = AXIS2_PLACEMENT_3D ( 'NONE', #5960, #5908, #7023 ) ;
#4278 = ORIENTED_EDGE ( 'NONE', *, *, #4901, .F. ) ;
#4279 = CARTESIAN_POINT ( 'NONE',  ( 0.000000000000000000, 20.41639017900859443, 4.916402349214656020 ) ) ;
#4280 = CARTESIAN_POINT ( 'NONE',  ( 1.250000000000000000, -6.429618962271402616, -1.000000000000000000 ) ) ;
#4281 = CARTESIAN_POINT ( 'NONE',  ( 4.999999999999999112, -13.09267581720863127, -5.622796541391703151 ) ) ;
#4282 = AXIS2_PLACEMENT_3D ( 'NONE', #3457, #3382, #1456 ) ;
#4283 = CYLINDRICAL_SURFACE ( 'NONE', #235, 21.00000000002100009 ) ;
#4284 = DIRECTION ( 'NONE',  ( -1.000000000000000000, 0.000000000000000000, 0.000000000000000000 ) ) ;
#4285 = ORIENTED_EDGE ( 'NONE', *, *, #6091, .T. ) ;
#4286 = FACE_OUTER_BOUND ( 'NONE', #11466, .T. ) ;
#4287 = ORIENTED_EDGE ( 'NONE', *, *, #11100, .T. ) ;
#4288 = DIRECTION ( 'NONE',  ( 0.000000000000000000, 0.8772744497699205279, 0.4799891038147466316 ) ) ;
#4289 = ORIENTED_EDGE ( 'NONE', *, *, #10196, .F. ) ;
#4290 = CARTESIAN_POINT ( 'NONE',  ( 4.999999999999999112, 0.000000000000000000, 20.24900000002024569 ) ) ;
#4291 = AXIS2_PLACEMENT_3D ( 'NONE', #10989, #5439, #9263 ) ;
#4292 = LINE ( 'NONE', #11906, #11931 ) ;
#4293 = ORIENTED_EDGE ( 'NONE', *, *, #11723, .F. ) ;
#4294 = LINE ( 'NONE', #11855, #6201 ) ;
#4295 = ADVANCED_FACE ( 'NONE', ( #5891 ), #358, .T. ) ;
#4296 = EDGE_LOOP ( 'NONE', ( #2120, #2578, #7552, #3563 ) ) ;
#4297 = CARTESIAN_POINT ( 'NONE',  ( 4.999999999999999112, 8.527191590521233877, -11.41582255376064126 ) ) ;
#4298 = VERTEX_POINT ( 'NONE', #1070 ) ;
#4299 = FACE_OUTER_BOUND ( 'NONE', #5904, .T. ) ;
#4300 = EDGE_LOOP ( 'NONE', ( #7317, #3974 ) ) ;
#4301 = DIRECTION ( 'NONE',  ( 0.000000000000000000, -1.000000000000000000, -0.000000000000000000 ) ) ;
#4302 = EDGE_CURVE ( 'NONE', #1460, #2942, #5068, .T. ) ;
#4303 = CARTESIAN_POINT ( 'NONE',  ( 0.000000000000000000, 0.000000000000000000, -1.000000000000000000 ) ) ;
#4304 = ADVANCED_FACE ( 'NONE', ( #7822 ), #5065, .F. ) ;
#4305 = CARTESIAN_POINT ( 'NONE',  ( 25.00000000000000000, 1.530808498934191521E-15, -12.50000000000000000 ) ) ;
#4306 = DIRECTION ( 'NONE',  ( 1.000000000000000000, -0.000000000000000000, -0.000000000000000000 ) ) ;
#4307 = DIRECTION ( 'NONE',  ( 0.000000000000000000, 0.000000000000000000, -1.000000000000000000 ) ) ;
#4308 = CARTESIAN_POINT ( 'NONE',  ( 4.999999999999999112, -11.41582255376079047, 8.527191590521034925 ) ) ;
#4309 = VERTEX_POINT ( 'NONE', #9644 ) ;
#4310 = ORIENTED_EDGE ( 'NONE', *, *, #4347, .F. ) ;
#4311 = PLANE ( 'NONE',  #10450 ) ;
#4312 =( LENGTH_UNIT ( ) NAMED_UNIT ( * ) SI_UNIT ( .MILLI., .METRE. ) );
#4313 = DIRECTION ( 'NONE',  ( 0.000000000000000000, 1.000000000000000000, 0.000000000000000000 ) ) ;
#4314 = ORIENTED_EDGE ( 'NONE', *, *, #7950, .T. ) ;
#4315 = CARTESIAN_POINT ( 'NONE',  ( -6.080745460913608902, 0.5192545390863924082, 0.000000000000000000 ) ) ;
#4316 = ORIENTED_EDGE ( 'NONE', *, *, #6114, .T. ) ;
#4317 = CARTESIAN_POINT ( 'NONE',  ( -1.400000000000001910, 0.000000000000000000, 0.000000000000000000 ) ) ;
#4318 = MANIFOLD_SOLID_BREP ( 'Body', #10567 ) ;
#4319 = ADVANCED_FACE ( 'NONE', ( #8944 ), #181, .T. ) ;
#4320 = EDGE_CURVE ( 'NONE', #5423, #5710, #2668, .T. ) ;
#4321 = ORIENTED_EDGE ( 'NONE', *, *, #3644, .F. ) ;
#4322 = ADVANCED_FACE ( 'NONE', ( #3000 ), #11731, .T. ) ;
#4323 = CYLINDRICAL_SURFACE ( 'NONE', #7804, 0.7499999999999997780 ) ;
#4324 = CARTESIAN_POINT ( 'NONE',  ( 70.79898987322334847, 3.500000000000001332, -45.49999999999998579 ) ) ;
#4325 = CARTESIAN_POINT ( 'NONE',  ( 20.00000000000000000, 1.530808498934191521E-15, -12.50000000000000000 ) ) ;
#4326 = CARTESIAN_POINT ( 'NONE',  ( 4.999999999999999112, -14.46592441914974891, 15.22291137398917193 ) ) ;
#4327 =( REPRESENTATION_RELATIONSHIP ('NONE','NONE', #9709, #7946 ) REPRESENTATION_RELATIONSHIP_WITH_TRANSFORMATION ( #8921 )SHAPE_REPRESENTATION_RELATIONSHIP( ) );
#4328 = VERTEX_POINT ( 'NONE', #6999 ) ;
#4329 = CARTESIAN_POINT ( 'NONE',  ( 2.500000000000000000, 1.178949249685213863, -2.042000000000001148 ) ) ;
#4330 = LINE ( 'NONE', #9689, #9226 ) ;
#4331 = VERTEX_POINT ( 'NONE', #2124 ) ;
#4332 = CARTESIAN_POINT ( 'NONE',  ( 4.999999999999999112, -22.83261415639512748, 14.41081992069301876 ) ) ;
#4333 = ORIENTED_EDGE ( 'NONE', *, *, #8691, .T. ) ;
#4334 = ADVANCED_FACE ( 'NONE', ( #249 ), #6068, .T. ) ;
#4335 = EDGE_CURVE ( 'NONE', #7138, #5192, #677, .T. ) ;
#4336 = DIRECTION ( 'NONE',  ( 0.000000000000000000, 0.000000000000000000, -1.000000000000000000 ) ) ;
#4337 = CYLINDRICAL_SURFACE ( 'NONE', #6991, 12.50000000000000000 ) ;
#4338 = CARTESIAN_POINT ( 'NONE',  ( 2.499999999999999556, 15.57980286237472711, 22.05152472667135655 ) ) ;
#4339 = CARTESIAN_POINT ( 'NONE',  ( 4.999999999999999112, 0.000000000000000000, 0.000000000000000000 ) ) ;
#4340 = DIRECTION ( 'NONE',  ( 0.000000000000000000, 0.000000000000000000, -1.000000000000000000 ) ) ;
#4341 = VERTEX_POINT ( 'NONE', #721 ) ;
#4342 = CARTESIAN_POINT ( 'NONE',  ( 0.000000000000000000, 20.18872947935930995, -1.561154383803291967 ) ) ;
#4343 = ORIENTED_EDGE ( 'NONE', *, *, #3578, .T. ) ;
#4344 = FILL_AREA_STYLE ('',( #5354 ) ) ;
#4345 = EDGE_LOOP ( 'NONE', ( #1018, #3584, #10775, #4368 ) ) ;
#4346 = DIRECTION ( 'NONE',  ( 0.000000000000000000, 0.000000000000000000, 1.000000000000000000 ) ) ;
#4347 = EDGE_CURVE ( 'NONE', #185, #4839, #6300, .T. ) ;
#4348 = DIRECTION ( 'NONE',  ( -1.000000000000000000, 0.000000000000000000, 0.000000000000000000 ) ) ;
#4349 = VERTEX_POINT ( 'NONE', #4534 ) ;
#4350 = DIRECTION ( 'NONE',  ( 0.000000000000000000, 0.000000000000000000, 1.000000000000000000 ) ) ;
#4351 = ORIENTED_EDGE ( 'NONE', *, *, #5142, .F. ) ;
#4352 = CARTESIAN_POINT ( 'NONE',  ( 0.000000000000000000, -2.791921004064099154, -22.37914155802288363 ) ) ;
#4353 = AXIS2_PLACEMENT_3D ( 'NONE', #1938, #1806, #8441 ) ;
#4354 = ORIENTED_EDGE ( 'NONE', *, *, #10735, .T. ) ;
#4355 = AXIS2_PLACEMENT_3D ( 'NONE', #3994, #8699, #121 ) ;
#4356 = AXIS2_PLACEMENT_3D ( 'NONE', #4456, #8332, #3389 ) ;
#4357 = DIRECTION ( 'NONE',  ( 0.000000000000000000, 0.9238795325112851842, 0.3826834323650938896 ) ) ;
#4358 = ADVANCED_BREP_SHAPE_REPRESENTATION ( '', ( #4548, #6056 ), #7232 ) ;
#4359 = ORIENTED_EDGE ( 'NONE', *, *, #2422, .T. ) ;
#4360 = CARTESIAN_POINT ( 'NONE',  ( 4.999999999999999112, -2.791921004064099154, -22.37914155802288363 ) ) ;
#4361 = AXIS2_PLACEMENT_3D ( 'NONE', #1415, #5240, #6244 ) ;
#4362 = AXIS2_PLACEMENT_3D ( 'NONE', #12047, #6254, #4491 ) ;
#4363 = FILL_AREA_STYLE ('',( #7132 ) ) ;
#4364 = LINE ( 'NONE', #11988, #8430 ) ;
#4365 = CARTESIAN_POINT ( 'NONE',  ( -15.00000000000000000, 40.00000000000000711, 2.000000000000000000 ) ) ;
#4366 = CARTESIAN_POINT ( 'NONE',  ( 43.00000000000000000, -2.941673623582830022, 4.043087470277766826 ) ) ;
#4367 = VERTEX_POINT ( 'NONE', #11223 ) ;
#4368 = ORIENTED_EDGE ( 'NONE', *, *, #6858, .T. ) ;
#4369 = ADVANCED_FACE ( 'NONE', ( #9245 ), #8351, .T. ) ;
#4370 = CARTESIAN_POINT ( 'NONE',  ( 0.8608560235772251268, -0.5999999999999993117, -3.803088852414125753 ) ) ;
#4371 = DIRECTION ( 'NONE',  ( 1.000000000000000000, -0.000000000000000000, -0.000000000000000000 ) ) ;
#4372 = VECTOR ( 'NONE', #6905, 1000.000000000000000 ) ;
#4373 = VERTEX_POINT ( 'NONE', #5488 ) ;
#4374 = CARTESIAN_POINT ( 'NONE',  ( 2.000000000000000000, -6.429618962271402616, 0.000000000000000000 ) ) ;
#4375 = AXIS2_PLACEMENT_3D ( 'NONE', #11115, #10246, #546 ) ;
#4376 = EDGE_CURVE ( 'NONE', #8845, #4298, #2075, .T. ) ;
#4377 = ORIENTED_EDGE ( 'NONE', *, *, #7000, .F. ) ;
#4378 = CARTESIAN_POINT ( 'NONE',  ( 3.309651814758564736, -5.455921364805393026, -1.000000000000000000 ) ) ;
#4379 = AXIS2_PLACEMENT_3D ( 'NONE', #11895, #9164, #7297 ) ;
#4380 = MANIFOLD_SOLID_BREP ( 'OuterRace', #5389 ) ;
#4381 = AXIS2_PLACEMENT_3D ( 'NONE', #8412, #5410, #3719 ) ;
#4382 = DIRECTION ( 'NONE',  ( -1.000000000000000000, -0.000000000000000000, 0.000000000000000000 ) ) ;
#4383 = CARTESIAN_POINT ( 'NONE',  ( 43.00000000000000000, 3.903127820947864496E-18, 0.000000000000000000 ) ) ;
#4384=STYLED_ITEM('',(#12391),#349);
#4385 = DIRECTION ( 'NONE',  ( -1.000000000000000000, 0.000000000000000000, -0.000000000000000000 ) ) ;
#4386 = CARTESIAN_POINT ( 'NONE',  ( 4.999999999999999112, -26.60936692326686881, -4.576198416197525098 ) ) ;
#4387 = EDGE_LOOP ( 'NONE', ( #11220, #2406, #3913, #8689 ) ) ;
#4388 = EDGE_CURVE ( 'NONE', #6632, #7160, #8466, .T. ) ;
#4389 = DIRECTION ( 'NONE',  ( 0.000000000000000000, 0.000000000000000000, 1.000000000000000000 ) ) ;
#4390 = FACE_OUTER_BOUND ( 'NONE', #10296, .T. ) ;
#4391 = VERTEX_POINT ( 'NONE', #1538 ) ;
#4392 = DIRECTION ( 'NONE',  ( 1.000000000000000000, 3.903127820947815962E-18, 0.000000000000000000 ) ) ;
#4393 = UNCERTAINTY_MEASURE_WITH_UNIT (LENGTH_MEASURE( 1.000000000000000082E-05 ), #513, 'distance_accuracy_value', 'NONE');
#4394 = EDGE_CURVE ( 'NONE', #4298, #8845, #11647, .T. ) ;
#4395 = CONTEXT_DEPENDENT_SHAPE_REPRESENTATION ( #7776, #5029 ) ;
#4396 = EDGE_CURVE ( 'NONE', #2794, #3713, #6269, .T. ) ;
#4397 = ORIENTED_EDGE ( 'NONE', *, *, #11406, .F. ) ;
#4398 = ADVANCED_FACE ( 'NONE', ( #7488 ), #8244, .T. ) ;
#4399 = VECTOR ( 'NONE', #5912, 1000.000000000000000 ) ;
#4400 = CIRCLE ( 'NONE', #7205, 20.24900000002024569 ) ;
#4401 = CARTESIAN_POINT ( 'NONE',  ( 4.999999999999999112, 0.000000000000000000, 0.000000000000000000 ) ) ;
#4402 = DIRECTION ( 'NONE',  ( -1.000000000000000000, 0.000000000000000000, 0.000000000000000000 ) ) ;
#4403 = PLANE ( 'NONE',  #10608 ) ;
#4404 = CYLINDRICAL_SURFACE ( 'NONE', #1429, 14.24900000001425227 ) ;
#4405 = DIRECTION ( 'NONE',  ( -1.000000000000000000, -0.000000000000000000, 0.000000000000000000 ) ) ;
#4406 = VERTEX_POINT ( 'NONE', #11284 ) ;
#4407 = AXIS2_PLACEMENT_3D ( 'NONE', #10353, #8498, #9196 ) ;
#4408 = CARTESIAN_POINT ( 'NONE',  ( 4.999999999999999112, 0.000000000000000000, 0.000000000000000000 ) ) ;
#4409 = AXIS2_PLACEMENT_3D ( 'NONE', #5979, #1287, #8983 ) ;
#4410 = ORIENTED_EDGE ( 'NONE', *, *, #434, .F. ) ;
#4411 =( NAMED_UNIT ( * ) PLANE_ANGLE_UNIT ( ) SI_UNIT ( $, .RADIAN. ) );
#4412 = SHAPE_REPRESENTATION_RELATIONSHIP ( 'NONE' , 'NONE' ,  #588, #6462 ) ;
#4413 = ORIENTED_EDGE ( 'NONE', *, *, #1027, .F. ) ;
#4414 = PLANE ( 'NONE',  #620 ) ;
#4415 = LINE ( 'NONE', #2482, #12147 ) ;
#4416 = VECTOR ( 'NONE', #10420, 1000.000000000000114 ) ;
#4417 = VECTOR ( 'NONE', #8972, 1000.000000000000000 ) ;
#4418 = CIRCLE ( 'NONE', #4210, 6.500000000000000888 ) ;
#4419 = VECTOR ( 'NONE', #7810, 1000.000000000000000 ) ;
#4420 = ORIENTED_EDGE ( 'NONE', *, *, #5405, .F. ) ;
#4421 = DIRECTION ( 'NONE',  ( 1.000000000000000000, 0.000000000000000000, 0.000000000000000000 ) ) ;
#4422 = VERTEX_POINT ( 'NONE', #1670 ) ;
#4423 = EDGE_CURVE ( 'NONE', #1692, #6339, #3278, .T. ) ;
#4424 = ADVANCED_FACE ( 'NONE', ( #5421 ), #10338, .T. ) ;
#4425 = DIRECTION ( 'NONE',  ( 0.000000000000000000, 0.000000000000000000, 1.000000000000000000 ) ) ;
#4426 = AXIS2_PLACEMENT_3D ( 'NONE', #6595, #9411, #11094 ) ;
#4427 = ORIENTED_EDGE ( 'NONE', *, *, #4498, .F. ) ;
#4428 = AXIS2_PLACEMENT_3D ( 'NONE', #11625, #1945, #10560 ) ;
#4429 = SURFACE_STYLE_USAGE ( .BOTH. , #1612 ) ;
#4430 = VECTOR ( 'NONE', #8538, 1000.000000000000000 ) ;
#4431 = AXIS2_PLACEMENT_3D ( 'NONE', #3756, #5826, #2077 ) ;
#4432 = CARTESIAN_POINT ( 'NONE',  ( 0.000000000000000000, 0.000000000000000000, 0.000000000000000000 ) ) ;
#4433 = ORIENTED_EDGE ( 'NONE', *, *, #3578, .F. ) ;
#4434 = CARTESIAN_POINT ( 'NONE',  ( 33.00000000000000000, 0.000000000000000000, 0.000000000000000000 ) ) ;
#4435 = PRESENTATION_LAYER_ASSIGNMENT (  '', '', ( #10815 ) ) ;
#4436 = AXIS2_PLACEMENT_3D ( 'NONE', #3339, #7914, #7966 ) ;
#4437 = AXIS2_PLACEMENT_3D ( 'NONE', #3821, #8514, #2055 ) ;
#4438 = CARTESIAN_POINT ( 'NONE',  ( 4.999999999999999112, 5.955107813822865914, -26.33508479058314222 ) ) ;
#4439 = AXIS2_PLACEMENT_3D ( 'NONE', #824, #7769, #7581 ) ;
#4440 = DIRECTION ( 'NONE',  ( -1.000000000000000000, 0.000000000000000000, -0.000000000000000000 ) ) ;
#4441 = CARTESIAN_POINT ( 'NONE',  ( 36.00000000000000711, 0.000000000000000000, -41.99999999999999289 ) ) ;
#4442 = DIRECTION ( 'NONE',  ( -1.000000000000000000, 0.000000000000000000, 0.000000000000000000 ) ) ;
#4443 = ORIENTED_EDGE ( 'NONE', *, *, #1497, .T. ) ;
#4444 = VERTEX_POINT ( 'NONE', #10871 ) ;
#4445 = DIRECTION ( 'NONE',  ( 0.000000000000000000, 0.000000000000000000, -1.000000000000000000 ) ) ;
#4446 =( NAMED_UNIT ( * ) PLANE_ANGLE_UNIT ( ) SI_UNIT ( $, .RADIAN. ) );
#4447 = LINE ( 'NONE', #3567, #10621 ) ;
#4448 = PRESENTATION_LAYER_ASSIGNMENT (  '', '', ( #7045 ) ) ;
#4449 = AXIS2_PLACEMENT_3D ( 'NONE', #11918, #3324, #6080 ) ;
#4450 = ORIENTED_EDGE ( 'NONE', *, *, #3023, .T. ) ;
#4451 = CARTESIAN_POINT ( 'NONE',  ( -20.00000000000000000, 40.00000000000000711, 12.50000000000000000 ) ) ;
#4452 = VECTOR ( 'NONE', #7486, 1000.000000000000000 ) ;
#4453 = TOROIDAL_SURFACE ( 'NONE', #3066, 6.250000000000000000, 0.7500000000000000000 ) ;
#4454 = ORIENTED_EDGE ( 'NONE', *, *, #9180, .T. ) ;
#4455 = DIRECTION ( 'NONE',  ( 0.000000000000000000, 0.000000000000000000, 1.000000000000000000 ) ) ;
#4456 = CARTESIAN_POINT ( 'NONE',  ( 4.999999999999999112, -16.90755573046745752, -0.4834863907627537372 ) ) ;
#4457 = EDGE_CURVE ( 'NONE', #1069, #2927, #10456, .T. ) ;
#4458 = CIRCLE ( 'NONE', #11045, 7.200000000007201528 ) ;
#4459 = CARTESIAN_POINT ( 'NONE',  ( 0.000000000000000000, 14.88411597386729213, 8.035066368449255592 ) ) ;
#4460 = DIRECTION ( 'NONE',  ( 1.000000000000000000, 0.000000000000000000, 0.000000000000000000 ) ) ;
#4461 = ORIENTED_EDGE ( 'NONE', *, *, #2329, .T. ) ;
#4462 = DIRECTION ( 'NONE',  ( 0.000000000000000000, 0.000000000000000000, -1.000000000000000000 ) ) ;
#4463 = CARTESIAN_POINT ( 'NONE',  ( 2.500000000000000444, -26.60936692326693631, 4.576198416197160057 ) ) ;
#4464 = VERTEX_POINT ( 'NONE', #3854 ) ;
#4465 = FACE_OUTER_BOUND ( 'NONE', #7723, .T. ) ;
#4466 = ORIENTED_EDGE ( 'NONE', *, *, #968, .T. ) ;
#4467 = AXIS2_PLACEMENT_3D ( 'NONE', #2251, #876, #4693 ) ;
#4468 = ADVANCED_FACE ( 'NONE', ( #5784 ), #6737, .T. ) ;
#4469 = CYLINDRICAL_SURFACE ( 'NONE', #8190, 2.700000000000000178 ) ;
#4470 = DIRECTION ( 'NONE',  ( -1.000000000000000000, -0.000000000000000000, -0.000000000000000000 ) ) ;
#4471 = EDGE_CURVE ( 'NONE', #6982, #1491, #2281, .T. ) ;
#4472 = DIRECTION ( 'NONE',  ( 0.000000000000000000, -0.3826834323650774028, -0.9238795325112918455 ) ) ;
#4474 = EDGE_CURVE ( 'NONE', #5247, #8156, #5074, .T. ) ;
#4473 = LINE ( 'NONE', #8296, #3234 ) ;
#4475 = ORIENTED_EDGE ( 'NONE', *, *, #9989, .F. ) ;
#4476 = CARTESIAN_POINT ( 'NONE',  ( 28.99999999999999645, 0.000000000000000000, -41.99999999999999289 ) ) ;
#4477 = ORIENTED_EDGE ( 'NONE', *, *, #10007, .F. ) ;
#4478 = CARTESIAN_POINT ( 'NONE',  ( 4.999999999999999112, 0.000000000000000000, 0.000000000000000000 ) ) ;
#4479 = DIRECTION ( 'NONE',  ( 1.000000000000000000, 0.000000000000000000, 0.000000000000000000 ) ) ;
#4480 = ORIENTED_EDGE ( 'NONE', *, *, #2679, .F. ) ;
#4481 = CARTESIAN_POINT ( 'NONE',  ( 37.00000000000000711, 0.000000000000000000, 0.000000000000000000 ) ) ;
#4482 = CARTESIAN_POINT ( 'NONE',  ( 20.00000000000000000, 0.000000000000000000, -25.00000000000000000 ) ) ;
#4483 = EDGE_CURVE ( 'NONE', #7385, #130, #9477, .T. ) ;
#4484 = VECTOR ( 'NONE', #5842, 1000.000000000000000 ) ;
#4485 = VERTEX_POINT ( 'NONE', #12333 ) ;
#4486 = CARTESIAN_POINT ( 'NONE',  ( -20.00000000000000000, 40.00000000000000711, 12.50000000000000000 ) ) ;
#4487 = EDGE_CURVE ( 'NONE', #2987, #3057, #11658, .T. ) ;
#4488 = EDGE_CURVE ( 'NONE', #10481, #2061, #9733, .T. ) ;
#4489 = EDGE_CURVE ( 'NONE', #558, #11181, #7791, .T. ) ;
#4490 = VERTEX_POINT ( 'NONE', #9675 ) ;
#4491 = DIRECTION ( 'NONE',  ( 1.000000000000000000, 0.000000000000000000, 0.000000000000000000 ) ) ;
#4492 = VERTEX_POINT ( 'NONE', #3783 ) ;
#4493 = VECTOR ( 'NONE', #4125, 1000.000000000000000 ) ;
#4494 =( NAMED_UNIT ( * ) PLANE_ANGLE_UNIT ( ) SI_UNIT ( $, .RADIAN. ) );
#4495 = CARTESIAN_POINT ( 'NONE',  ( 29.00000000000000000, 0.000000000000000000, -41.99999999999999289 ) ) ;
#4496 = VERTEX_POINT ( 'NONE', #3969 ) ;
#4497 = DIRECTION ( 'NONE',  ( 0.000000000000000000, 0.000000000000000000, 1.000000000000000000 ) ) ;
#4498 = EDGE_CURVE ( 'NONE', #11527, #4496, #4783, .T. ) ;
#4499 = EDGE_CURVE ( 'NONE', #4951, #3355, #10593, .T. ) ;
#4500 = CARTESIAN_POINT ( 'NONE',  ( 37.00000000000000711, 6.123233995736765296E-16, -5.000000000000000000 ) ) ;
#4501 = CIRCLE ( 'NONE', #11086, 0.1000000000000002554 ) ;
#4502 = CARTESIAN_POINT ( 'NONE',  ( 36.00000000000000711, 1.456773409934505593E-31, -41.99999999999998579 ) ) ;
#4503 = DIRECTION ( 'NONE',  ( 1.000000000000000000, -0.000000000000000000, -0.000000000000000000 ) ) ;
#4504 = ORIENTED_EDGE ( 'NONE', *, *, #11106, .T. ) ;
#4505 = ORIENTED_EDGE ( 'NONE', *, *, #4582, .F. ) ;
#4506 = FACE_OUTER_BOUND ( 'NONE', #9159, .T. ) ;
#4507 = PRESENTATION_STYLE_ASSIGNMENT (( #11072 ) ) ;
#4508 = DIRECTION ( 'NONE',  ( 1.000000000000000000, 0.000000000000000000, 0.000000000000000000 ) ) ;
#4509 = ORIENTED_EDGE ( 'NONE', *, *, #6191, .F. ) ;
#4510 = CYLINDRICAL_SURFACE ( 'NONE', #4282, 9.600000000009600853 ) ;
#4511 = ORIENTED_EDGE ( 'NONE', *, *, #7750, .F. ) ;
#4512 = DIRECTION ( 'NONE',  ( -1.000000000000000000, -0.000000000000000000, -0.000000000000000000 ) ) ;
#4513 = CARTESIAN_POINT ( 'NONE',  ( 4.999999999999999112, -9.168210874537443544, -18.05452603534175537 ) ) ;
#4514 = FACE_OUTER_BOUND ( 'NONE', #11785, .T. ) ;
#4515 = ORIENTED_EDGE ( 'NONE', *, *, #10522, .T. ) ;
#4516 = LINE ( 'NONE', #6466, #8844 ) ;
#4517 = FACE_OUTER_BOUND ( 'NONE', #8619, .T. ) ;
#4518 = ORIENTED_EDGE ( 'NONE', *, *, #3548, .T. ) ;
#4519 = LINE ( 'NONE', #9157, #6973 ) ;
#4520 = CARTESIAN_POINT ( 'NONE',  ( 4.999999999999999112, 0.4834863907625768231, 16.90755573046746463 ) ) ;
#4521 = EDGE_LOOP ( 'NONE', ( #8180, #11265, #910, #2539 ) ) ;
#4522 = CARTESIAN_POINT ( 'NONE',  ( 4.999999999999999112, 0.000000000000000000, 0.000000000000000000 ) ) ;
#4523 = UNCERTAINTY_MEASURE_WITH_UNIT (LENGTH_MEASURE( 1.000000000000000082E-05 ), #4965, 'distance_accuracy_value', 'NONE');
#4524 = ORIENTED_EDGE ( 'NONE', *, *, #1119, .F. ) ;
#4525 =( LENGTH_UNIT ( ) NAMED_UNIT ( * ) SI_UNIT ( .MILLI., .METRE. ) );
#4526 = FACE_OUTER_BOUND ( 'NONE', #9415, .T. ) ;
#4527 = DIRECTION ( 'NONE',  ( 0.000000000000000000, 0.000000000000000000, -1.000000000000000000 ) ) ;
#4528 = CARTESIAN_POINT ( 'NONE',  ( 4.999999999999999112, 0.000000000000000000, 0.000000000000000000 ) ) ;
#4529 = CARTESIAN_POINT ( 'NONE',  ( 4.999999999999999112, 5.984728032765264771, -21.74405275335751853 ) ) ;
#4530 = ORIENTED_EDGE ( 'NONE', *, *, #2803, .T. ) ;
#4531 = ORIENTED_EDGE ( 'NONE', *, *, #10127, .T. ) ;
#4532 = DIRECTION ( 'NONE',  ( 0.000000000000000000, 0.3826834323650905589, -0.9238795325112864054 ) ) ;
#4533 = ORIENTED_EDGE ( 'NONE', *, *, #10179, .F. ) ;
#4534 = CARTESIAN_POINT ( 'NONE',  ( 0.000000000000000000, -20.13931372320384128, -5.950465759859079995 ) ) ;
#4535 = EDGE_CURVE ( 'NONE', #11534, #2088, #284, .T. ) ;
#4536 = CARTESIAN_POINT ( 'NONE',  ( 37.00000000000000711, 2.168404344971008868E-16, -41.99999999999998579 ) ) ;
#4537 = ORIENTED_EDGE ( 'NONE', *, *, #8612, .F. ) ;
#4538 = CYLINDRICAL_SURFACE ( 'NONE', #2802, 7.200000000007202416 ) ;
#4539 = EDGE_CURVE ( 'NONE', #7704, #7924, #1282, .T. ) ;
#4540 = CARTESIAN_POINT ( 'NONE',  ( 37.00000000000000711, -2.432816653220593039, 4.137801726981678030 ) ) ;
#4541 = ORIENTED_EDGE ( 'NONE', *, *, #3569, .F. ) ;
#4542 = FACE_OUTER_BOUND ( 'NONE', #7228, .T. ) ;
#4543 = ORIENTED_EDGE ( 'NONE', *, *, #484, .F. ) ;
#4544 = CYLINDRICAL_SURFACE ( 'NONE', #4577, 0.7499999999999997780 ) ;
#4545 = EDGE_LOOP ( 'NONE', ( #11290, #4676, #2938, #9438, #627, #12295, #924, #1160, #4454, #2984, #10958, #1987 ) ) ;
#4546 = ADVANCED_FACE ( 'NONE', ( #7734, #11523 ), #2968, .T. ) ;
#4547 =( NAMED_UNIT ( * ) SI_UNIT ( $, .STERADIAN. ) SOLID_ANGLE_UNIT ( ) );
#4548 = MANIFOLD_SOLID_BREP ( 'Boss-Extrude3', #6364 ) ;
#4549 = DIRECTION ( 'NONE',  ( 0.000000000000000000, 0.8772744497699203059, 0.4799891038147465760 ) ) ;
#4550 = ADVANCED_FACE ( 'NONE', ( #8866 ), #2043, .T. ) ;
#4552 = ORIENTED_EDGE ( 'NONE', *, *, #1171, .T. ) ;
#4551 = EDGE_CURVE ( 'NONE', #5359, #4145, #5676, .T. ) ;
#4553 = CARTESIAN_POINT ( 'NONE',  ( 4.999999999999999112, 26.33508479058320617, 5.955107813822601237 ) ) ;
#4554 = EDGE_CURVE ( 'NONE', #344, #11586, #8887, .T. ) ;
#4555 = DIRECTION ( 'NONE',  ( 0.000000000000000000, 0.000000000000000000, 1.000000000000000000 ) ) ;
#4556 = CIRCLE ( 'NONE', #2759, 7.200000000007202416 ) ;
#4557 = AXIS2_PLACEMENT_3D ( 'NONE', #208, #3286, #7857 ) ;
#4558 = DIRECTION ( 'NONE',  ( -1.000000000000000000, -0.000000000000000000, -0.000000000000000000 ) ) ;
#4559 = DIRECTION ( 'NONE',  ( -1.000000000000000000, 0.000000000000000000, 0.000000000000000000 ) ) ;
#4560 = ORIENTED_EDGE ( 'NONE', *, *, #2283, .T. ) ;
#4561 = ORIENTED_EDGE ( 'NONE', *, *, #1102, .T. ) ;
#4562 = CARTESIAN_POINT ( 'NONE',  ( 46.00000000000000000, -3.499999999999998668, -38.49999999999998579 ) ) ;
#4563 = EDGE_CURVE ( 'NONE', #6113, #10112, #3483, .T. ) ;
#4564 = CARTESIAN_POINT ( 'NONE',  ( -5.686050877451574337, -5.768780236673276995, -1.000000000000000000 ) ) ;
#4565 = DIRECTION ( 'NONE',  ( -1.000000000000000000, 0.000000000000000000, -0.000000000000000000 ) ) ;
#4566 = ORIENTED_EDGE ( 'NONE', *, *, #12168, .T. ) ;
#4567 = DIRECTION ( 'NONE',  ( 0.000000000000000000, 0.6828850436591806794, 0.7305258497456466049 ) ) ;
#4568 = AXIS2_PLACEMENT_3D ( 'NONE', #8403, #6285, #7153 ) ;
#4569 =( REPRESENTATION_RELATIONSHIP ('NONE','NONE', #9709, #8907 ) REPRESENTATION_RELATIONSHIP_WITH_TRANSFORMATION ( #9734 )SHAPE_REPRESENTATION_RELATIONSHIP( ) );
#4570 = AXIS2_PLACEMENT_3D ( 'NONE', #6264, #10078, #5320 ) ;
#4571 = LINE ( 'NONE', #8331, #10381 ) ;
#4572 = DIRECTION ( 'NONE',  ( 0.000000000000000000, 0.000000000000000000, 1.000000000000000000 ) ) ;
#4573 = VERTEX_POINT ( 'NONE', #6153 ) ;
#4574 = DIRECTION ( 'NONE',  ( -1.000000000000000000, -0.000000000000000000, -0.000000000000000000 ) ) ;
#4575 = DIRECTION ( 'NONE',  ( 0.000000000000000000, 0.000000000000000000, 1.000000000000000000 ) ) ;
#4576 = AXIS2_PLACEMENT_3D ( 'NONE', #11417, #5978, #9684 ) ;
#4577 = AXIS2_PLACEMENT_3D ( 'NONE', #11108, #3497, #7318 ) ;
#4578 = ORIENTED_EDGE ( 'NONE', *, *, #1629, .T. ) ;
#4579 = CYLINDRICAL_SURFACE ( 'NONE', #4568, 2.149999999999999023 ) ;
#4580 = EDGE_CURVE ( 'NONE', #3417, #9895, #9793, .T. ) ;
#4581 = DIRECTION ( 'NONE',  ( 0.000000000000000000, 0.000000000000000000, -1.000000000000000000 ) ) ;
#4582 = EDGE_CURVE ( 'NONE', #1798, #238, #10465, .T. ) ;
#4583 = VECTOR ( 'NONE', #2103, 1000.000000000000000 ) ;
#4584 = VERTEX_POINT ( 'NONE', #8920 ) ;
#4585 = CARTESIAN_POINT ( 'NONE',  ( 17.00000000000000000, 0.000000000000000000, 0.000000000000000000 ) ) ;
#4586 = ORIENTED_EDGE ( 'NONE', *, *, #8092, .F. ) ;
#4587 = DIRECTION ( 'NONE',  ( 0.000000000000000000, 1.000000000000000000, -1.471414886128461471E-15 ) ) ;
#4588=STYLED_ITEM('',(#12377),#313);
#4589 = DIRECTION ( 'NONE',  ( 0.1305261922200524616, 0.9914448613738103822, -0.000000000000000000 ) ) ;
#4590 = CARTESIAN_POINT ( 'NONE',  ( 29.00000000000000000, 9.184850993605147944E-16, -49.49999999999999289 ) ) ;
#4591 = DIRECTION ( 'NONE',  ( 0.000000000000000000, 0.000000000000000000, 1.000000000000000000 ) ) ;
#4592 = CYLINDRICAL_SURFACE ( 'NONE', #3039, 5.750000000000000000 ) ;
#4593 = ORIENTED_EDGE ( 'NONE', *, *, #9578, .F. ) ;
#4594 = VERTEX_POINT ( 'NONE', #1334 ) ;
#4595 = CYLINDRICAL_SURFACE ( 'NONE', #7223, 27.00000000002699707 ) ;
#4596 = AXIS2_PLACEMENT_3D ( 'NONE', #8211, #2565, #7285 ) ;
#4597 = ORIENTED_EDGE ( 'NONE', *, *, #11230, .F. ) ;
#4598 = DIRECTION ( 'NONE',  ( -1.000000000000000000, 0.000000000000000000, 0.000000000000000000 ) ) ;
#4599 = DIRECTION ( 'NONE',  ( 0.000000000000000000, -1.000000000000000000, 0.000000000000000000 ) ) ;
#4600 = ORIENTED_EDGE ( 'NONE', *, *, #2031, .T. ) ;
#4601 = CIRCLE ( 'NONE', #3403, 20.24900000002024569 ) ;
#4602 = LINE ( 'NONE', #6682, #6605 ) ;
#4603 = CARTESIAN_POINT ( 'NONE',  ( 2.499999999999999556, 26.60936692326690789, -4.576198416197345686 ) ) ;
#4604 = AXIS2_PLACEMENT_3D ( 'NONE', #7782, #4026, #4955 ) ;
#4605 = VERTEX_POINT ( 'NONE', #1215 ) ;
#4606 = CARTESIAN_POINT ( 'NONE',  ( 2.354826896168714434, -6.962563485461402024, 0.000000000000000000 ) ) ;
#4607 = ADVANCED_FACE ( 'NONE', ( #6971, #7919 ), #10777, .T. ) ;
#4608 = AXIS2_PLACEMENT_3D ( 'NONE', #7714, #5571, #11315 ) ;
#4609 = CIRCLE ( 'NONE', #5811, 9.600000000009600853 ) ;
#4610 = CARTESIAN_POINT ( 'NONE',  ( 0.8603041673727119809, 0.5999999999999998668, 3.802994432158365967 ) ) ;
#4611 = ADVANCED_FACE ( 'NONE', ( #282, #1394, #215 ), #2214, .F. ) ;
#4612 = VERTEX_POINT ( 'NONE', #6102 ) ;
#4613 = CYLINDRICAL_SURFACE ( 'NONE', #9970, 5.750000000000000000 ) ;
#4614 = ORIENTED_EDGE ( 'NONE', *, *, #593, .T. ) ;
#4615 =( LENGTH_UNIT ( ) NAMED_UNIT ( * ) SI_UNIT ( .MILLI., .METRE. ) );
#4616 = CIRCLE ( 'NONE', #3816, 4.800000000000000711 ) ;
#4617 = DIRECTION ( 'NONE',  ( -1.000000000000000000, 0.000000000000000000, 0.000000000000000000 ) ) ;
#4618 = CIRCLE ( 'NONE', #617, 2.041999999999999815 ) ;
#4619 = PRODUCT_DEFINITION_SHAPE ( 'NONE', 'NONE',  #7780 ) ;
#4620 = CIRCLE ( 'NONE', #7227, 7.200000000007202416 ) ;
#4621 = VERTEX_POINT ( 'NONE', #9864 ) ;
#4622 = CYLINDRICAL_SURFACE ( 'NONE', #4353, 5.199999999999996625 ) ;
#4623 = AXIS2_PLACEMENT_3D ( 'NONE', #10104, #715, #4527 ) ;
#4624 = CARTESIAN_POINT ( 'NONE',  ( 2.500000000000000000, -1.178949249685213863, 2.042000000000002924 ) ) ;
#4625 = ADVANCED_FACE ( 'NONE', ( #4207 ), #7043, .F. ) ;
#4626 = STYLED_ITEM ( 'NONE', ( #1750 ), #7062 ) ;
#4627 = CIRCLE ( 'NONE', #4216, 40.00000000000000711 ) ;
#4628 = VECTOR ( 'NONE', #6512, 1000.000000000000000 ) ;
#4629 = EDGE_CURVE ( 'NONE', #3527, #4033, #7864, .T. ) ;
#4630 = CIRCLE ( 'NONE', #5831, 7.200000000007204193 ) ;
#4631 = DIRECTION ( 'NONE',  ( 1.000000000000000000, -0.000000000000000000, 0.000000000000000000 ) ) ;
#4632 = CARTESIAN_POINT ( 'NONE',  ( 20.00000000000000000, 0.000000000000000000, 0.000000000000000000 ) ) ;
#4633 = ADVANCED_FACE ( 'NONE', ( #10720 ), #5211, .F. ) ;
#4634 = EDGE_LOOP ( 'NONE', ( #8679, #8427, #1517, #3160 ) ) ;
#4635 = ORIENTED_EDGE ( 'NONE', *, *, #10732, .F. ) ;
#4636 = CARTESIAN_POINT ( 'NONE',  ( -36.00000000000000711, 0.000000000000000000, -7.500000000000000888 ) ) ;
#4637 = CARTESIAN_POINT ( 'NONE',  ( 14.39999999999999680, 2.449293598294706414E-16, -2.000000000000000000 ) ) ;
#4638 = CARTESIAN_POINT ( 'NONE',  ( 33.00000000000000000, 0.000000000000000000, -41.99999999999999289 ) ) ;
#4639 = VERTEX_POINT ( 'NONE', #4276 ) ;
#4640 = CARTESIAN_POINT ( 'NONE',  ( -1.400000000000000133, 6.245698675651501825E-16, 5.100000000000000533 ) ) ;
#4641 = COLOUR_RGB ( '',1.000000000000000000, 0.9490196078431372140, 0.9098039215686274384 ) ;
#4642 = AXIS2_PLACEMENT_3D ( 'NONE', #2032, #4029, #209 ) ;
#4643 = AXIS2_PLACEMENT_3D ( 'NONE', #11780, #345, #476 ) ;
#4644 = CIRCLE ( 'NONE', #9640, 5.000000000000000000 ) ;
#4645 = MANIFOLD_SOLID_BREP ( 'Mirror2', #2988 ) ;
#4646 = CARTESIAN_POINT ( 'NONE',  ( 0.000000000000000000, 4.916402349214583190, 20.41639017900861219 ) ) ;
#4647 = ORIENTED_EDGE ( 'NONE', *, *, #11800, .T. ) ;
#4648 = AXIS2_PLACEMENT_3D ( 'NONE', #8066, #6302, #11962 ) ;
#4649 = LINE ( 'NONE', #8468, #242 ) ;
#4650 = DIRECTION ( 'NONE',  ( 1.000000000000000000, 0.000000000000000000, 0.000000000000000000 ) ) ;
#4651 = ORIENTED_EDGE ( 'NONE', *, *, #10946, .T. ) ;
#4652 = DIRECTION ( 'NONE',  ( -1.000000000000000000, -0.000000000000000000, -0.000000000000000000 ) ) ;
#4653 = CIRCLE ( 'NONE', #6058, 6.500000000000000888 ) ;
#4654 = DIRECTION ( 'NONE',  ( 1.000000000000000000, 1.734723475976807094E-16, 0.000000000000000000 ) ) ;
#4655 = ORIENTED_EDGE ( 'NONE', *, *, #6727, .T. ) ;
#4656 = DIRECTION ( 'NONE',  ( 1.000000000000000000, 1.734723475976807094E-16, 0.000000000000000000 ) ) ;
#4657 = VERTEX_POINT ( 'NONE', #1281 ) ;
#4658 = EDGE_CURVE ( 'NONE', #2990, #7961, #3088, .T. ) ;
#4659 = CIRCLE ( 'NONE', #3464, 4.799999999999998934 ) ;
#4660 = PLANE ( 'NONE',  #4989 ) ;
#4661 = EDGE_CURVE ( 'NONE', #5533, #2913, #2648, .T. ) ;
#4662 = CYLINDRICAL_SURFACE ( 'NONE', #7193, 4.799999999999998934 ) ;
#4663 = CARTESIAN_POINT ( 'NONE',  ( -36.00000000000000711, 0.000000000000000000, 0.000000000000000000 ) ) ;
#4664 = DIRECTION ( 'NONE',  ( 0.000000000000000000, 0.7512545167371323940, -0.6600126143355578012 ) ) ;
#4665 = DIRECTION ( 'NONE',  ( 0.000000000000000000, -1.000000000000000000, 0.000000000000000000 ) ) ;
#4666 = ORIENTED_EDGE ( 'NONE', *, *, #4244, .F. ) ;
#4667 = ORIENTED_EDGE ( 'NONE', *, *, #4471, .T. ) ;
#4668 = DIRECTION ( 'NONE',  ( 0.000000000000000000, 0.000000000000000000, 1.000000000000000000 ) ) ;
#4669 = ORIENTED_EDGE ( 'NONE', *, *, #4712, .T. ) ;
#4670 = DIRECTION ( 'NONE',  ( 0.000000000000000000, 0.000000000000000000, 1.000000000000000000 ) ) ;
#4671 = DIRECTION ( 'NONE',  ( 0.000000000000000000, 0.000000000000000000, 1.000000000000000000 ) ) ;
#4672 = VERTEX_POINT ( 'NONE', #11089 ) ;
#4673 = LINE ( 'NONE', #9358, #10609 ) ;
#4674 = DIRECTION ( 'NONE',  ( 0.000000000000000000, 0.000000000000000000, -1.000000000000000000 ) ) ;
#4675 = ORIENTED_EDGE ( 'NONE', *, *, #1658, .T. ) ;
#4676 = ORIENTED_EDGE ( 'NONE', *, *, #2653, .T. ) ;
#4677 = DIRECTION ( 'NONE',  ( 0.000000000000000000, 0.000000000000000000, -1.000000000000000000 ) ) ;
#4678 = CARTESIAN_POINT ( 'NONE',  ( 28.99999999999999645, 0.000000000000000000, -41.99999999999999289 ) ) ;
#4679 = FACE_OUTER_BOUND ( 'NONE', #9548, .T. ) ;
#4680 = VERTEX_POINT ( 'NONE', #1527 ) ;
#4681 = FACE_OUTER_BOUND ( 'NONE', #12214, .T. ) ;
#4682 = ORIENTED_EDGE ( 'NONE', *, *, #6242, .T. ) ;
#4683 = PLANE ( 'NONE',  #3505 ) ;
#4684 = CONICAL_SURFACE ( 'NONE', #7295, 2.055000000000000160, 0.7853981633974633780 ) ;
#4685 = ORIENTED_EDGE ( 'NONE', *, *, #9868, .F. ) ;
#4686 = DIRECTION ( 'NONE',  ( 1.000000000000000000, 0.000000000000000000, 0.000000000000000000 ) ) ;
#4687 = DIRECTION ( 'NONE',  ( 1.000000000000000000, 0.000000000000000000, 0.000000000000000000 ) ) ;
#4688 = AXIS2_PLACEMENT_3D ( 'NONE', #12065, #628, #745 ) ;
#4689 = CYLINDRICAL_SURFACE ( 'NONE', #2974, 21.00000000002100009 ) ;
#4690 = CARTESIAN_POINT ( 'NONE',  ( 43.00000000000000000, 0.000000000000000000, 0.000000000000000000 ) ) ;
#4691 = VERTEX_POINT ( 'NONE', #1766 ) ;
#4692 = ORIENTED_EDGE ( 'NONE', *, *, #2253, .F. ) ;
#4693 = DIRECTION ( 'NONE',  ( 0.000000000000000000, 0.4999999999999948375, 0.8660254037844415942 ) ) ;
#4694 = DIRECTION ( 'NONE',  ( -1.000000000000000000, -0.000000000000000000, -0.000000000000000000 ) ) ;
#4695 = CARTESIAN_POINT ( 'NONE',  ( 4.999999999999999112, 14.41081992069340600, -22.83261415639488234 ) ) ;
#4696 = ADVANCED_FACE ( 'NONE', ( #4465 ), #1583, .F. ) ;
#4697 = ORIENTED_EDGE ( 'NONE', *, *, #11492, .T. ) ;
#4698 = CYLINDRICAL_SURFACE ( 'NONE', #1586, 4.800000000000000711 ) ;
#4699 = EDGE_CURVE ( 'NONE', #3546, #10829, #1685, .T. ) ;
#4700 = AXIS2_PLACEMENT_3D ( 'NONE', #1614, #11113, #544 ) ;
#4701 = DIRECTION ( 'NONE',  ( 0.000000000000000000, 0.000000000000000000, 1.000000000000000000 ) ) ;
#4702 = FACE_OUTER_BOUND ( 'NONE', #8390, .T. ) ;
#4703 = DIRECTION ( 'NONE',  ( -1.000000000000000000, 0.000000000000000000, 0.000000000000000000 ) ) ;
#4704 = CARTESIAN_POINT ( 'NONE',  ( 20.00000000000000000, 44.00000000000002132, 12.50000000000000000 ) ) ;
#4705 = ORIENTED_EDGE ( 'NONE', *, *, #12169, .T. ) ;
#4706 = DIRECTION ( 'NONE',  ( -1.000000000000000000, 0.000000000000000000, 0.000000000000000000 ) ) ;
#4707 = PLANE ( 'NONE',  #6031 ) ;
#4708 = EDGE_LOOP ( 'NONE', ( #10926, #949, #3162, #9172 ) ) ;
#4709 = DIRECTION ( 'NONE',  ( -1.000000000000000000, -0.000000000000000000, -0.000000000000000000 ) ) ;
#4710 = ORIENTED_EDGE ( 'NONE', *, *, #3810, .T. ) ;
#4711 = EDGE_CURVE ( 'NONE', #5214, #6431, #9677, .T. ) ;
#4712 = EDGE_CURVE ( 'NONE', #866, #3677, #10254, .T. ) ;
#4713 = EDGE_CURVE ( 'NONE', #10072, #6450, #6477, .T. ) ;
#4714 = FILL_AREA_STYLE ('',( #6009 ) ) ;
#4715 = DIRECTION ( 'NONE',  ( -1.000000000000000000, -0.000000000000000000, -0.000000000000000000 ) ) ;
#4716 = CARTESIAN_POINT ( 'NONE',  ( 4.999999999999999112, 14.88411597386729213, 8.035066368449255592 ) ) ;
#4717 = LINE ( 'NONE', #12083, #7038 ) ;
#4718 = CARTESIAN_POINT ( 'NONE',  ( 37.00000000000000711, 1.456773409934505593E-31, -41.99999999999998579 ) ) ;
#4719 = VERTEX_POINT ( 'NONE', #4332 ) ;
#4720 = VERTEX_POINT ( 'NONE', #760 ) ;
#4721 = CARTESIAN_POINT ( 'NONE',  ( 15.00000000000000355, 40.00000000000000711, 0.000000000000000000 ) ) ;
#4722 = VERTEX_POINT ( 'NONE', #10211 ) ;
#4724 = B_SPLINE_CURVE_WITH_KNOTS ( 'NONE', 3,
 ( #10018, #4370, #505, #8322, #2444, #8200, #1451, #5451, #5381, #12113 ),
 .UNSPECIFIED., .F., .F.,
 ( 4, 2, 2, 2, 4 ),
 ( 0.007142761454519953000, 0.007565713830041730613, 0.007988666205563509093, 0.008411618581085286706, 0.008834570956607064318 ),
 .UNSPECIFIED. ) ;
#4723 = DIRECTION ( 'NONE',  ( -0.000000000000000000, 1.000000000000000000, -0.000000000000000000 ) ) ;
#4725 = SHAPE_DEFINITION_REPRESENTATION ( #1131, #1080 ) ;
#4726 = ADVANCED_FACE ( 'NONE', ( #12131 ), #8223, .T. ) ;
#4727 = ORIENTED_EDGE ( 'NONE', *, *, #2933, .T. ) ;
#4728 = CARTESIAN_POINT ( 'NONE',  ( 1.199999999999999956, 0.000000000000000000, 0.000000000000000000 ) ) ;
#4729 = FACE_OUTER_BOUND ( 'NONE', #10137, .T. ) ;
#4730 = EDGE_LOOP ( 'NONE', ( #11973, #10708 ) ) ;
#4731 = ORIENTED_EDGE ( 'NONE', *, *, #8882, .T. ) ;
#4732 = DIRECTION ( 'NONE',  ( 0.000000000000000000, 0.000000000000000000, 1.000000000000000000 ) ) ;
#4733 = CARTESIAN_POINT ( 'NONE',  ( 27.38165010660258503, 0.8169585525225424583, -43.25800585191812075 ) ) ;
#4734 = DIRECTION ( 'NONE',  ( -1.000000000000000000, -0.000000000000000000, 0.000000000000000000 ) ) ;
#4735 = ORIENTED_EDGE ( 'NONE', *, *, #6391, .T. ) ;
#4736 = CARTESIAN_POINT ( 'NONE',  ( -33.00000000000000000, 0.000000000000000000, 0.000000000000000000 ) ) ;
#4737 = ORIENTED_EDGE ( 'NONE', *, *, #5956, .T. ) ;
#4738 = APPLICATION_CONTEXT ( 'automotive_design' ) ;
#4739 = EDGE_CURVE ( 'NONE', #3605, #12289, #11664, .T. ) ;
#4740 = ORIENTED_EDGE ( 'NONE', *, *, #8490, .F. ) ;
#4741 = CARTESIAN_POINT ( 'NONE',  ( 36.00000000000000000, 3.061616997868380183E-16, -39.49999999999999289 ) ) ;
#4742 = ORIENTED_EDGE ( 'NONE', *, *, #887, .F. ) ;
#4743 = DIRECTION ( 'NONE',  ( -1.000000000000000000, 0.000000000000000000, -0.000000000000000000 ) ) ;
#4744 = FACE_OUTER_BOUND ( 'NONE', #11269, .T. ) ;
#4745 = DIRECTION ( 'NONE',  ( 0.000000000000000000, 1.000000000000000000, 3.373073425507084106E-15 ) ) ;
#4746 = DIRECTION ( 'NONE',  ( -1.000000000000000000, -0.000000000000000000, -0.000000000000000000 ) ) ;
#4747 = VERTEX_POINT ( 'NONE', #3528 ) ;
#4748 = ORIENTED_EDGE ( 'NONE', *, *, #4023, .T. ) ;
#4749 = LINE ( 'NONE', #8571, #6459 ) ;
#4750 =( NAMED_UNIT ( * ) PLANE_ANGLE_UNIT ( ) SI_UNIT ( $, .RADIAN. ) );
#4751 = DIRECTION ( 'NONE',  ( -1.000000000000000000, -0.000000000000000000, 0.000000000000000000 ) ) ;
#4752 = CARTESIAN_POINT ( 'NONE',  ( -31.74999999999995737, 0.000000000000000000, 2.500000000000000444 ) ) ;
#4753 = ORIENTED_EDGE ( 'NONE', *, *, #6406, .F. ) ;
#4754 = CARTESIAN_POINT ( 'NONE',  ( 37.00000000000000711, 4.886001309506331935, -37.03844870997966154 ) ) ;
#4755 = VECTOR ( 'NONE', #6463, 1000.000000000000000 ) ;
#4756 = CARTESIAN_POINT ( 'NONE',  ( 45.00000000000001421, 5.744562646538025952, -46.00000000000000000 ) ) ;
#4757 = ADVANCED_FACE ( 'NONE', ( #1710 ), #6343, .T. ) ;
#4758 = CARTESIAN_POINT ( 'NONE',  ( 0.000000000000000000, -13.17168466712917585, -15.37949036966225513 ) ) ;
#4759 = LINE ( 'NONE', #81, #10038 ) ;
#4760 = VERTEX_POINT ( 'NONE', #9290 ) ;
#4761 = EDGE_CURVE ( 'NONE', #4099, #10051, #6893, .T. ) ;
#4762 = DIRECTION ( 'NONE',  ( 1.000000000000000000, 0.000000000000000000, 0.000000000000000000 ) ) ;
#4763 = CARTESIAN_POINT ( 'NONE',  ( 1.500000000000001332, 0.000000000000000000, 0.000000000000000000 ) ) ;
#4764 = AXIS2_PLACEMENT_3D ( 'NONE', #1439, #11982, #3438 ) ;
#4765 = ORIENTED_EDGE ( 'NONE', *, *, #2720, .T. ) ;
#4766 = FACE_OUTER_BOUND ( 'NONE', #9935, .T. ) ;
#4767 = CIRCLE ( 'NONE', #6363, 9.600000000009600853 ) ;
#4768 = ORIENTED_EDGE ( 'NONE', *, *, #9434, .F. ) ;
#4769 = CARTESIAN_POINT ( 'NONE',  ( -26.00000000000000355, 0.000000000000000000, 6.500000000000000888 ) ) ;
#4770 = DIRECTION ( 'NONE',  ( 0.000000000000000000, 0.000000000000000000, 1.000000000000000000 ) ) ;
#4771 = PLANE ( 'NONE',  #1770 ) ;
#4772 = AXIS2_PLACEMENT_3D ( 'NONE', #5284, #6877, #4205 ) ;
#4773 = EDGE_CURVE ( 'NONE', #7692, #6998, #9291, .T. ) ;
#4774 = VECTOR ( 'NONE', #581, 1000.000000000000000 ) ;
#4775 = CARTESIAN_POINT ( 'NONE',  ( 0.1481481481481481122, -4.797713218419819903, -1.000000000000000000 ) ) ;
#4776 = DIRECTION ( 'NONE',  ( 0.000000000000000000, -1.000000000000000000, 0.000000000000000000 ) ) ;
#4777 = EDGE_LOOP ( 'NONE', ( #8731, #1721 ) ) ;
#4779 = EDGE_CURVE ( 'NONE', #4040, #4422, #1892, .T. ) ;
#4778 = ORIENTED_EDGE ( 'NONE', *, *, #2037, .T. ) ;
#4780 = DIRECTION ( 'NONE',  ( 0.000000000000000000, 0.000000000000000000, 1.000000000000000000 ) ) ;
#4781 = EDGE_CURVE ( 'NONE', #3968, #4059, #3657, .T. ) ;
#4782 = VERTEX_POINT ( 'NONE', #3839 ) ;
#4783 = LINE ( 'NONE', #8672, #4075 ) ;
#4784 =( NAMED_UNIT ( * ) SI_UNIT ( $, .STERADIAN. ) SOLID_ANGLE_UNIT ( ) );
#4785 = ORIENTED_EDGE ( 'NONE', *, *, #666, .T. ) ;
#4786 = AXIS2_PLACEMENT_3D ( 'NONE', #9950, #2136, #3148 ) ;
#4787 = VECTOR ( 'NONE', #4887, 1000.000000000000000 ) ;
#4788 = DIRECTION ( 'NONE',  ( -1.000000000000000000, -0.000000000000000000, -0.000000000000000000 ) ) ;
#4789 = CIRCLE ( 'NONE', #3992, 4.799999999999999822 ) ;
#4790 = ORIENTED_EDGE ( 'NONE', *, *, #5097, .T. ) ;
#4791 = EDGE_LOOP ( 'NONE', ( #3791, #6174, #10394, #3647 ) ) ;
#4792 = CARTESIAN_POINT ( 'NONE',  ( 51.00000000000000000, -3.499999999999998668, -38.49999999999998579 ) ) ;
#4793 = DIRECTION ( 'NONE',  ( 0.000000000000000000, 0.000000000000000000, 1.000000000000000000 ) ) ;
#4794 = DIRECTION ( 'NONE',  ( 0.000000000000000000, 0.000000000000000000, 1.000000000000000000 ) ) ;
#4795 = DIRECTION ( 'NONE',  ( -0.000000000000000000, 1.000000000000000000, -0.000000000000000000 ) ) ;
#4796 = VECTOR ( 'NONE', #11473, 1000.000000000000000 ) ;
#4797 = ORIENTED_EDGE ( 'NONE', *, *, #3568, .F. ) ;
#4798 = CIRCLE ( 'NONE', #11770, 5.000000000000004441 ) ;
#4799 = CARTESIAN_POINT ( 'NONE',  ( 4.999999999999997335, 4.769696007084728073, -1.500000000000000000 ) ) ;
#4800 = ORIENTED_EDGE ( 'NONE', *, *, #11048, .T. ) ;
#4801 = ORIENTED_EDGE ( 'NONE', *, *, #12102, .T. ) ;
#4802 = DIRECTION ( 'NONE',  ( -1.000000000000000000, 0.000000000000000000, 0.000000000000000000 ) ) ;
#4803 = ORIENTED_EDGE ( 'NONE', *, *, #7002, .F. ) ;
#4804 = DIRECTION ( 'NONE',  ( 1.000000000000000000, 0.000000000000000000, 0.000000000000000000 ) ) ;
#4805 = AXIS2_PLACEMENT_3D ( 'NONE', #1967, #90, #10660 ) ;
#4806 = CIRCLE ( 'NONE', #8812, 2.000000000000000000 ) ;
#4807 = DIRECTION ( 'NONE',  ( 0.000000000000000000, -0.7071067811865389130, -0.7071067811865562325 ) ) ;
#4808 = EDGE_CURVE ( 'NONE', #114, #3280, #11, .T. ) ;
#4809 = EDGE_CURVE ( 'NONE', #10227, #6613, #292, .T. ) ;
#4810 = CARTESIAN_POINT ( 'NONE',  ( 1.000000000000000000, -0.6000000000000001998, 3.826895796574397046 ) ) ;
#4811 = LINE ( 'NONE', #5558, #9259 ) ;
#4812 = ORIENTED_EDGE ( 'NONE', *, *, #1269, .T. ) ;
#4813 = CARTESIAN_POINT ( 'NONE',  ( 4.999999999999999112, 5.955107813822506202, 26.33508479058322393 ) ) ;
#4814 = ADVANCED_BREP_SHAPE_REPRESENTATION ( '', ( #4318, #6056 ), #3638 ) ;
#4815 = VECTOR ( 'NONE', #12084, 1000.000000000000000 ) ;
#4816 = CARTESIAN_POINT ( 'NONE',  ( 4.999999999999999112, -14.40062958310459251, -1.672489362011137404 ) ) ;
#4817 = CIRCLE ( 'NONE', #2814, 9.600000000009600853 ) ;
#4818 = CARTESIAN_POINT ( 'NONE',  ( 51.00000000000000000, -3.499999999999998668, -45.49999999999998579 ) ) ;
#4819 = ORIENTED_EDGE ( 'NONE', *, *, #12183, .F. ) ;
#4820 = FACE_OUTER_BOUND ( 'NONE', #2975, .T. ) ;
#4821 = STYLED_ITEM ( 'NONE', ( #5747 ), #4358 ) ;
#4822 = CIRCLE ( 'NONE', #222, 27.00000000002699707 ) ;
#4823 = AXIS2_PLACEMENT_3D ( 'NONE', #9, #9586, #9660 ) ;
#4824 = AXIS2_PLACEMENT_3D ( 'NONE', #6789, #5663, #2033 ) ;
#4825 = VECTOR ( 'NONE', #4058, 1000.000000000000000 ) ;
#4826 = CARTESIAN_POINT ( 'NONE',  ( 2.500000000000000000, 0.000000000000000000, 0.000000000000000000 ) ) ;
#4827 = CARTESIAN_POINT ( 'NONE',  ( 37.00000000000000711, -3.403685371105885427, -38.61548734756097190 ) ) ;
#4828 = CYLINDRICAL_SURFACE ( 'NONE', #7854, 0.7500000000000000000 ) ;
#4829 = DIRECTION ( 'NONE',  ( 0.000000000000000000, -1.000000000000000000, 0.000000000000000000 ) ) ;
#4830 = VERTEX_POINT ( 'NONE', #1903 ) ;
#4831 = CARTESIAN_POINT ( 'NONE',  ( 4.999999999999999112, 0.000000000000000000, 0.000000000000000000 ) ) ;
#4832 = DIRECTION ( 'NONE',  ( -1.000000000000000000, -0.000000000000000000, 0.000000000000000000 ) ) ;
#4833 = MECHANICAL_DESIGN_GEOMETRIC_PRESENTATION_REPRESENTATION (  '', ( #5039 ), #2631 ) ;
#4834 = AXIS2_PLACEMENT_3D ( 'NONE', #3033, #22, #1913 ) ;
#4835 = ORIENTED_EDGE ( 'NONE', *, *, #4808, .F. ) ;
#4836 = CARTESIAN_POINT ( 'NONE',  ( -36.00100000000000477, 6.368163355566235395E-16, -36.79999999999999716 ) ) ;
#4837 = CIRCLE ( 'NONE', #424, 20.24900000002024569 ) ;
#4838 = AXIS2_PLACEMENT_3D ( 'NONE', #1760, #7219, #2459 ) ;
#4839 = VERTEX_POINT ( 'NONE', #9405 ) ;
#4840 = EDGE_CURVE ( 'NONE', #2049, #8321, #8893, .T. ) ;
#4841 = AXIS2_PLACEMENT_3D ( 'NONE', #3305, #8245, #6168 ) ;
#4842 = AXIS2_PLACEMENT_3D ( 'NONE', #1010, #943, #195 ) ;
#4843 = AXIS2_PLACEMENT_3D ( 'NONE', #11042, #2344, #3414 ) ;
#4844 = FACE_OUTER_BOUND ( 'NONE', #5735, .T. ) ;
#4845 = DIRECTION ( 'NONE',  ( 1.000000000000000000, -0.000000000000000000, 0.000000000000000000 ) ) ;
#4846 = CIRCLE ( 'NONE', #258, 7.000000000000000000 ) ;
#4847 = LINE ( 'NONE', #2961, #3837 ) ;
#4848 = CARTESIAN_POINT ( 'NONE',  ( 20.00000000000000000, 44.00000000000002132, 12.50000000000000000 ) ) ;
#4849 = ORIENTED_EDGE ( 'NONE', *, *, #447, .T. ) ;
#4850 = ORIENTED_EDGE ( 'NONE', *, *, #10117, .T. ) ;
#4851 = ORIENTED_EDGE ( 'NONE', *, *, #9712, .F. ) ;
#4852 = DIRECTION ( 'NONE',  ( 1.000000000000000000, -0.000000000000000000, 0.000000000000000000 ) ) ;
#4853 = ITEM_DEFINED_TRANSFORMATION ( 'NONE', 'NONE', #8053,  #6056 ) ;
#4854 = VERTEX_POINT ( 'NONE', #9662 ) ;
#4855 = VECTOR ( 'NONE', #6842, 1000.000000000000000 ) ;
#4856 = ADVANCED_FACE ( 'NONE', ( #5582 ), #4684, .T. ) ;
#4857 = AXIS2_PLACEMENT_3D ( 'NONE', #7387, #11182, #2624 ) ;
#4858 = EDGE_CURVE ( 'NONE', #4914, #11321, #896, .T. ) ;
#4859 = EDGE_LOOP ( 'NONE', ( #2673, #8874, #4157, #1564 ) ) ;
#4860 = EDGE_CURVE ( 'NONE', #2662, #1975, #10872, .T. ) ;
#4861 = EDGE_LOOP ( 'NONE', ( #4851, #3306, #2199, #11836 ) ) ;
#4862 = CARTESIAN_POINT ( 'NONE',  ( 4.999999999999999112, -20.18872947935932061, 1.561154383803151191 ) ) ;
#4863 = CARTESIAN_POINT ( 'NONE',  ( 50.00005079999999680, 0.000000000000000000, 1.500000000000000000 ) ) ;
#4864 = DIRECTION ( 'NONE',  ( -1.000000000000000000, -0.000000000000000000, -0.000000000000000000 ) ) ;
#4865 = FACE_OUTER_BOUND ( 'NONE', #2528, .T. ) ;
#4866 = ORIENTED_EDGE ( 'NONE', *, *, #11922, .F. ) ;
#4867 = AXIS2_PLACEMENT_3D ( 'NONE', #7306, #2531, #6353 ) ;
#4868 = FACE_OUTER_BOUND ( 'NONE', #2466, .T. ) ;
#4869 = ORIENTED_EDGE ( 'NONE', *, *, #2634, .T. ) ;
#4870 = EDGE_LOOP ( 'NONE', ( #11730, #4923, #272, #7599 ) ) ;
#4871 = DIRECTION ( 'NONE',  ( -1.000000000000000000, 0.000000000000000000, -0.000000000000000000 ) ) ;
#4872 = ORIENTED_EDGE ( 'NONE', *, *, #1649, .F. ) ;
#4873 = DIRECTION ( 'NONE',  ( 0.000000000000000000, 0.000000000000000000, 1.000000000000000000 ) ) ;
#4874 = EDGE_CURVE ( 'NONE', #3510, #5352, #3021, .T. ) ;
#4875 = EDGE_CURVE ( 'NONE', #4594, #12228, #7093, .T. ) ;
#4876 = EDGE_CURVE ( 'NONE', #4373, #6551, #1016, .T. ) ;
#4877 = LINE ( 'NONE', #10437, #12166 ) ;
#4878 = ORIENTED_EDGE ( 'NONE', *, *, #11375, .T. ) ;
#4879 = DIRECTION ( 'NONE',  ( 1.000000000000000000, 0.000000000000000000, 0.000000000000000000 ) ) ;
#4880 = LINE ( 'NONE', #8700, #10836 ) ;
#4881 = EDGE_LOOP ( 'NONE', ( #4990, #895, #10528, #12116 ) ) ;
#4882 = AXIS2_PLACEMENT_3D ( 'NONE', #8659, #3904, #2955 ) ;
#4883 = DIRECTION ( 'NONE',  ( 0.000000000000000000, 0.000000000000000000, 1.000000000000000000 ) ) ;
#4884 = LINE ( 'NONE', #4752, #8698 ) ;
#4885 = ADVANCED_FACE ( 'NONE', ( #4766 ), #8589, .T. ) ;
#4886 = ORIENTED_EDGE ( 'NONE', *, *, #11777, .T. ) ;
#4887 = DIRECTION ( 'NONE',  ( 1.000000000000000000, 0.000000000000000000, 0.000000000000000000 ) ) ;
#4888 = EDGE_CURVE ( 'NONE', #7044, #10239, #10259, .T. ) ;
#4889 = VECTOR ( 'NONE', #11322, 1000.000000000000000 ) ;
#4890 = DIRECTION ( 'NONE',  ( 0.000000000000000000, 0.000000000000000000, 1.000000000000000000 ) ) ;
#4891 = CARTESIAN_POINT ( 'NONE',  ( 0.2500000000000002220, 0.000000000000000000, 0.000000000000000000 ) ) ;
#4892 = CARTESIAN_POINT ( 'NONE',  ( 4.999999999999999112, 19.24938187143305512, -6.283573709965099674 ) ) ;
#4893 = CARTESIAN_POINT ( 'NONE',  ( 5.200000000000002842, 0.000000000000000000, 0.000000000000000000 ) ) ;
#4894 = ORIENTED_EDGE ( 'NONE', *, *, #3566, .F. ) ;
#4895 = DIRECTION ( 'NONE',  ( 0.000000000000000000, 0.000000000000000000, 1.000000000000000000 ) ) ;
#4896 = CARTESIAN_POINT ( 'NONE',  ( -20.00000000000000000, 40.00000000000000711, 12.50000000000000000 ) ) ;
#4897 = EDGE_LOOP ( 'NONE', ( #2375, #11782, #3930, #11070 ) ) ;
#4898 = DIRECTION ( 'NONE',  ( 0.000000000000000000, -0.9238795325112826307, -0.3826834323650997183 ) ) ;
#4899 = UNCERTAINTY_MEASURE_WITH_UNIT (LENGTH_MEASURE( 1.000000000000000082E-05 ), #1293, 'distance_accuracy_value', 'NONE');
#4900 = VECTOR ( 'NONE', #11734, 1000.000000000000000 ) ;
#4901 = EDGE_CURVE ( 'NONE', #2661, #11627, #11510, .T. ) ;
#4902 = ORIENTED_EDGE ( 'NONE', *, *, #10762, .T. ) ;
#4903 = FACE_OUTER_BOUND ( 'NONE', #2595, .T. ) ;
#4904 = LINE ( 'NONE', #7595, #2359 ) ;
#4905 = DIRECTION ( 'NONE',  ( -1.000000000000000000, 0.000000000000000000, 0.000000000000000000 ) ) ;
#4906 = PLANE ( 'NONE',  #7238 ) ;
#4907 = ORIENTED_EDGE ( 'NONE', *, *, #7563, .T. ) ;
#4908 = VERTEX_POINT ( 'NONE', #2024 ) ;
#4909 = CARTESIAN_POINT ( 'NONE',  ( -10.00000000000000000, 0.000000000000000000, 0.000000000000000000 ) ) ;
#4910 = EDGE_LOOP ( 'NONE', ( #4675, #8408, #7842, #9900 ) ) ;
#4911 = FILL_AREA_STYLE ('',( #1919 ) ) ;
#4912 = CONTEXT_DEPENDENT_SHAPE_REPRESENTATION ( #10316, #7252 ) ;
#4913 = ORIENTED_EDGE ( 'NONE', *, *, #2505, .F. ) ;
#4914 = VERTEX_POINT ( 'NONE', #10655 ) ;
#4915 = ORIENTED_EDGE ( 'NONE', *, *, #3102, .T. ) ;
#4916 = CARTESIAN_POINT ( 'NONE',  ( -1.500000000000001332, 0.000000000000000000, 0.000000000000000000 ) ) ;
#4917 = CARTESIAN_POINT ( 'NONE',  ( -20.00000000000000000, 44.00000000000001421, 12.50000000000000000 ) ) ;
#4918 = CARTESIAN_POINT ( 'NONE',  ( -6.080745460913608902, 0.5192545390863924082, -1.000000000000000000 ) ) ;
#4919 = DIRECTION ( 'NONE',  ( -1.000000000000000000, -0.000000000000000000, -0.000000000000000000 ) ) ;
#4920 = ADVANCED_FACE ( 'NONE', ( #6775 ), #6850, .F. ) ;
#4921 = ORIENTED_EDGE ( 'NONE', *, *, #7592, .F. ) ;
#4922 = DIRECTION ( 'NONE',  ( 0.000000000000000000, 0.000000000000000000, -1.000000000000000000 ) ) ;
#4923 = ORIENTED_EDGE ( 'NONE', *, *, #9584, .F. ) ;
#4924 = EDGE_CURVE ( 'NONE', #5416, #11746, #5493, .T. ) ;
#4925 = ORIENTED_EDGE ( 'NONE', *, *, #10277, .T. ) ;
#4926 = CARTESIAN_POINT ( 'NONE',  ( 43.00000000000000000, 3.903127820947864496E-18, 0.000000000000000000 ) ) ;
#4927 = ORIENTED_EDGE ( 'NONE', *, *, #5322, .T. ) ;
#4928 = CARTESIAN_POINT ( 'NONE',  ( 0.000000000000000000, 19.24938187143305512, -6.283573709965099674 ) ) ;
#4929 = DIRECTION ( 'NONE',  ( 0.000000000000000000, 1.000000000000000000, 0.000000000000000000 ) ) ;
#4930 = EDGE_CURVE ( 'NONE', #1981, #536, #6697, .T. ) ;
#4931 = ORIENTED_EDGE ( 'NONE', *, *, #10613, .T. ) ;
#4932 = CARTESIAN_POINT ( 'NONE',  ( 0.000000000000000000, 19.60720892790252989, 11.14352537685181588 ) ) ;
#4933 = CARTESIAN_POINT ( 'NONE',  ( 10.00000000000000000, 44.00000000000001421, 12.50000000000000000 ) ) ;
#4934 = VERTEX_POINT ( 'NONE', #7589 ) ;
#4935 = CARTESIAN_POINT ( 'NONE',  ( 50.00005079999999680, 6.799999999999999822, -1.500000000000000000 ) ) ;
#4936 = EDGE_CURVE ( 'NONE', #11041, #9485, #3714, .T. ) ;
#4937 = DIRECTION ( 'NONE',  ( 0.000000000000000000, 0.000000000000000000, 1.000000000000000000 ) ) ;
#4938 = ADVANCED_FACE ( 'NONE', ( #142, #3956 ), #7528, .F. ) ;
#4939 = ADVANCED_FACE ( 'NONE', ( #8960 ), #203, .F. ) ;
#4940 = DIRECTION ( 'NONE',  ( -1.000000000000000000, 0.000000000000000000, 0.000000000000000000 ) ) ;
#4941 = VERTEX_POINT ( 'NONE', #3331 ) ;
#4942 = LINE ( 'NONE', #5370, #7987 ) ;
#4943 = DIRECTION ( 'NONE',  ( 0.000000000000000000, 0.000000000000000000, 1.000000000000000000 ) ) ;
#4944 = CARTESIAN_POINT ( 'NONE',  ( 29.00000000000000000, 0.000000000000000000, -41.99999999999999289 ) ) ;
#4945 = EDGE_CURVE ( 'NONE', #3376, #5880, #1288, .T. ) ;
#4946 = CYLINDRICAL_SURFACE ( 'NONE', #8256, 5.000000000000000000 ) ;
#4947 = CARTESIAN_POINT ( 'NONE',  ( 2.499999999999999556, 22.83261415639523051, -14.41081992069285178 ) ) ;
#4948 = ORIENTED_EDGE ( 'NONE', *, *, #8595, .T. ) ;
#4949 = CARTESIAN_POINT ( 'NONE',  ( 28.99999999999999645, 0.000000000000000000, -47.19999999999998863 ) ) ;
#4950 = CARTESIAN_POINT ( 'NONE',  ( 42.00000000000000000, 1.908195823574506293E-17, -41.99999999999998579 ) ) ;
#4951 = VERTEX_POINT ( 'NONE', #8846 ) ;
#4952 = PLANE ( 'NONE',  #3686 ) ;
#4953 = ORIENTED_EDGE ( 'NONE', *, *, #2422, .F. ) ;
#4954 = DIRECTION ( 'NONE',  ( 0.000000000000000000, 0.000000000000000000, 1.000000000000000000 ) ) ;
#4955 = DIRECTION ( 'NONE',  ( 0.000000000000000000, 0.000000000000000000, 1.000000000000000000 ) ) ;
#4956 = LINE ( 'NONE', #9908, #8564 ) ;
#4957 = EDGE_CURVE ( 'NONE', #6377, #10347, #2681, .T. ) ;
#4958 = ADVANCED_FACE ( 'NONE', ( #11822 ), #1321, .T. ) ;
#4959 = DIRECTION ( 'NONE',  ( 0.000000000000000000, 0.000000000000000000, 1.000000000000000000 ) ) ;
#4960 = FACE_OUTER_BOUND ( 'NONE', #7354, .T. ) ;
#4961 = CIRCLE ( 'NONE', #5363, 9.600000000009604406 ) ;
#4962 = EDGE_LOOP ( 'NONE', ( #10356, #4586, #3122, #2808 ) ) ;
#4963 = AXIS2_PLACEMENT_3D ( 'NONE', #4663, #903, #8480 ) ;
#4964 = ORIENTED_EDGE ( 'NONE', *, *, #4483, .F. ) ;
#4965 =( LENGTH_UNIT ( ) NAMED_UNIT ( * ) SI_UNIT ( .MILLI., .METRE. ) );
#4966 = CONTEXT_DEPENDENT_SHAPE_REPRESENTATION ( #4569, #4232 ) ;
#4967 = ORIENTED_EDGE ( 'NONE', *, *, #5306, .T. ) ;
#4968 = AXIS2_PLACEMENT_3D ( 'NONE', #598, #10114, #5492 ) ;
#4969 =( REPRESENTATION_RELATIONSHIP ('NONE','NONE', #9709, #588 ) REPRESENTATION_RELATIONSHIP_WITH_TRANSFORMATION ( #2465 )SHAPE_REPRESENTATION_RELATIONSHIP( ) );
#4970 = CIRCLE ( 'NONE', #1775, 27.00000000002699707 ) ;
#4971 = DIRECTION ( 'NONE',  ( 0.000000000000000000, 0.000000000000000000, 1.000000000000000000 ) ) ;
#4972 = ORIENTED_EDGE ( 'NONE', *, *, #1755, .T. ) ;
#4973 = DIRECTION ( 'NONE',  ( 1.000000000000000000, 0.000000000000000000, 0.000000000000000000 ) ) ;
#4974 = CARTESIAN_POINT ( 'NONE',  ( 45.00000000000000000, 6.123233995736765296E-16, -5.000000000000000000 ) ) ;
#4975 = CARTESIAN_POINT ( 'NONE',  ( 50.00005079999999680, 0.000000000000000000, 0.000000000000000000 ) ) ;
#4976 = FACE_OUTER_BOUND ( 'NONE', #332, .T. ) ;
#4977 = ORIENTED_EDGE ( 'NONE', *, *, #3902, .F. ) ;
#4978 = CIRCLE ( 'NONE', #7182, 6.500000000000000888 ) ;
#4979 = ORIENTED_EDGE ( 'NONE', *, *, #5424, .T. ) ;
#4980 = AXIS2_PLACEMENT_3D ( 'NONE', #3557, #7324, #6442 ) ;
#4981 = EDGE_LOOP ( 'NONE', ( #9110, #3659, #2026 ) ) ;
#4982 = AXIS2_PLACEMENT_3D ( 'NONE', #9869, #5528, #11036 ) ;
#4983 = CARTESIAN_POINT ( 'NONE',  ( -36.00000000000000000, 0.000000000000000000, 0.000000000000000000 ) ) ;
#4984 = ORIENTED_EDGE ( 'NONE', *, *, #1906, .F. ) ;
#4985 = DIRECTION ( 'NONE',  ( -1.000000000000000000, 0.000000000000000000, 0.000000000000000000 ) ) ;
#4986 = AXIS2_PLACEMENT_3D ( 'NONE', #4916, #4973, #6871 ) ;
#4987 = CARTESIAN_POINT ( 'NONE',  ( 37.00000000000000711, 1.456773409934505593E-31, -41.99999999999998579 ) ) ;
#4988 = EDGE_CURVE ( 'NONE', #2927, #1069, #9685, .T. ) ;
#4989 = AXIS2_PLACEMENT_3D ( 'NONE', #10521, #5771, #6668 ) ;
#4990 = ORIENTED_EDGE ( 'NONE', *, *, #10346, .F. ) ;
#4991 = CARTESIAN_POINT ( 'NONE',  ( 0.000000000000000000, 0.000000000000000000, 0.000000000000000000 ) ) ;
#4992 = CARTESIAN_POINT ( 'NONE',  ( 2.500000000000000000, 2.357898499370433054, -1.951563910473907981E-15 ) ) ;
#4993 = ORIENTED_EDGE ( 'NONE', *, *, #10277, .F. ) ;
#4994 = DIRECTION ( 'NONE',  ( 0.000000000000000000, 0.000000000000000000, 1.000000000000000000 ) ) ;
#4995 = DIRECTION ( 'NONE',  ( 0.000000000000000000, 0.000000000000000000, 1.000000000000000000 ) ) ;
#4996 = COLOUR_RGB ( '',1.000000000000000000, 0.9490196078431372140, 0.9098039215686274384 ) ;
#4997 = CARTESIAN_POINT ( 'NONE',  ( 2.499999999999999556, 15.22291137398942418, -14.46592441914948779 ) ) ;
#4998 = VECTOR ( 'NONE', #5515, 999.9999999999998863 ) ;
#4999 = VERTEX_POINT ( 'NONE', #8909 ) ;
#5000 = CARTESIAN_POINT ( 'NONE',  ( 14.39999999999999680, 0.000000000000000000, 2.000000000000000000 ) ) ;
#5001 = VECTOR ( 'NONE', #7751, 1000.000000000000000 ) ;
#5002 = ADVANCED_FACE ( 'NONE', ( #321 ), #2139, .T. ) ;
#5003 = EDGE_CURVE ( 'NONE', #8570, #6497, #6025, .T. ) ;
#5004 = ADVANCED_FACE ( 'NONE', ( #1142 ), #7143, .T. ) ;
#5005 = AXIS2_PLACEMENT_3D ( 'NONE', #6192, #1445, #12227 ) ;
#5006 = SURFACE_STYLE_USAGE ( .BOTH. , #440 ) ;
#5007 = CARTESIAN_POINT ( 'NONE',  ( -36.00000000000000000, 0.000000000000000000, 5.000000000000000000 ) ) ;
#5008 = CIRCLE ( 'NONE', #6418, 7.200000000007201528 ) ;
#5009 = DIRECTION ( 'NONE',  ( -1.000000000000000000, 0.000000000000000000, -0.000000000000000000 ) ) ;
#5010 = CARTESIAN_POINT ( 'NONE',  ( 4.999999999999999112, 0.000000000000000000, 0.000000000000000000 ) ) ;
#5011 = EDGE_LOOP ( 'NONE', ( #5534, #6800, #10442, #1956 ) ) ;
#5012 = CARTESIAN_POINT ( 'NONE',  ( 36.00000000000000711, 1.456773409934505593E-31, -41.99999999999998579 ) ) ;
#5013 = CARTESIAN_POINT ( 'NONE',  ( 0.000000000000000000, 0.000000000000000000, 0.000000000000000000 ) ) ;
#5014 = ORIENTED_EDGE ( 'NONE', *, *, #3855, .F. ) ;
#5015 = CARTESIAN_POINT ( 'NONE',  ( 33.00000000000000000, 0.000000000000000000, -41.99999999999999289 ) ) ;
#5016 = VERTEX_POINT ( 'NONE', #2087 ) ;
#5017 = LINE ( 'NONE', #3283, #9037 ) ;
#5018 = AXIS2_PLACEMENT_3D ( 'NONE', #5797, #8683, #10785 ) ;
#5019 = AXIS2_PLACEMENT_3D ( 'NONE', #8740, #3981, #12315 ) ;
#5020 = VECTOR ( 'NONE', #6928, 1000.000000000000000 ) ;
#5021 = CIRCLE ( 'NONE', #10407, 7.200000000007204193 ) ;
#5022 = EDGE_CURVE ( 'NONE', #11273, #2049, #11465, .T. ) ;
#5023 = LINE ( 'NONE', #1324, #7200 ) ;
#5024 = DIRECTION ( 'NONE',  ( -1.000000000000000000, -0.000000000000000000, -0.000000000000000000 ) ) ;
#5025 = CYLINDRICAL_SURFACE ( 'NONE', #1040, 4.000000000000003553 ) ;
#5026 = CARTESIAN_POINT ( 'NONE',  ( 4.999999999999999112, 21.74405275335758247, 5.984728032765037398 ) ) ;
#5027 = CIRCLE ( 'NONE', #1637, 7.500000000000000888 ) ;
#5028 = CIRCLE ( 'NONE', #9426, 40.00000000000000711 ) ;
#5029 = PRODUCT_DEFINITION_SHAPE ( 'NONE', 'NONE',  #12367 ) ;
#5030 = ORIENTED_EDGE ( 'NONE', *, *, #7502, .F. ) ;
#5031 = AXIS2_PLACEMENT_3D ( 'NONE', #9171, #2527, #3598 ) ;
#5032 = SURFACE_STYLE_USAGE ( .BOTH. , #961 ) ;
#5033 = VERTEX_POINT ( 'NONE', #5082 ) ;
#5034 = FILL_AREA_STYLE_COLOUR ( '', #8675 ) ;
#5035 = PRODUCT_CONTEXT ( 'NONE', #10489, 'mechanical' ) ;
#5036 = ORIENTED_EDGE ( 'NONE', *, *, #2712, .T. ) ;
#5037 = ADVANCED_FACE ( 'NONE', ( #11697, #7090 ), #4952, .T. ) ;
#5038 = ADVANCED_FACE ( 'NONE', ( #6958, #452 ), #10835, .F. ) ;
#5039 = STYLED_ITEM ( 'NONE', ( #3174 ), #7504 ) ;
#5040 = VECTOR ( 'NONE', #10703, 1000.000000000000000 ) ;
#5041 = AXIS2_PLACEMENT_3D ( 'NONE', #7825, #3753, #6647 ) ;
#5042 = AXIS2_PLACEMENT_3D ( 'NONE', #6283, #3582, #7401 ) ;
#5043 = CARTESIAN_POINT ( 'NONE',  ( -1.250000000000000000, -6.429618962271402616, -1.000000000000000000 ) ) ;
#5044 = VERTEX_POINT ( 'NONE', #2268 ) ;
#5045 = DIRECTION ( 'NONE',  ( 0.000000000000000000, 0.000000000000000000, 1.000000000000000000 ) ) ;
#5046 = FACE_OUTER_BOUND ( 'NONE', #1474, .T. ) ;
#5047 = DIRECTION ( 'NONE',  ( -1.000000000000000000, -0.000000000000000000, -0.000000000000000000 ) ) ;
#5048 = PLANE ( 'NONE',  #11595 ) ;
#5049 = VERTEX_POINT ( 'NONE', #10709 ) ;
#5050 =( GEOMETRIC_REPRESENTATION_CONTEXT ( 3 ) GLOBAL_UNCERTAINTY_ASSIGNED_CONTEXT ( ( #143 ) ) GLOBAL_UNIT_ASSIGNED_CONTEXT ( ( #8122, #2478, #7308 ) ) REPRESENTATION_CONTEXT ( 'NONE', 'WORKASPACE' ) );
#5051 = AXIS2_PLACEMENT_3D ( 'NONE', #10882, #6131, #2620 ) ;
#5052 = ORIENTED_EDGE ( 'NONE', *, *, #8087, .F. ) ;
#5053 = AXIS2_PLACEMENT_3D ( 'NONE', #4909, #11580, #6735 ) ;
#5054 =( NAMED_UNIT ( * ) SI_UNIT ( $, .STERADIAN. ) SOLID_ANGLE_UNIT ( ) );
#5055 = CIRCLE ( 'NONE', #4241, 2.700000000000000622 ) ;
#5056 = EDGE_LOOP ( 'NONE', ( #11298, #3125, #1942, #7788 ) ) ;
#5057 = CARTESIAN_POINT ( 'NONE',  ( 43.00000000000000000, 0.000000000000000000, 0.000000000000000000 ) ) ;
#5058 = DIRECTION ( 'NONE',  ( 0.000000000000000000, 0.000000000000000000, 1.000000000000000000 ) ) ;
#5059 = CYLINDRICAL_SURFACE ( 'NONE', #4, 5.000000000000000000 ) ;
#5060 = CIRCLE ( 'NONE', #8871, 20.24900000002024569 ) ;
#5061 = ORIENTED_EDGE ( 'NONE', *, *, #5701, .T. ) ;
#5062 = CARTESIAN_POINT ( 'NONE',  ( -5.686050877451574337, -5.768780236673276995, 0.000000000000000000 ) ) ;
#5063 = LINE ( 'NONE', #2070, #267 ) ;
#5064 = ORIENTED_EDGE ( 'NONE', *, *, #8383, .T. ) ;
#5065 = CYLINDRICAL_SURFACE ( 'NONE', #8073, 4.799999999999999822 ) ;
#5066 = CARTESIAN_POINT ( 'NONE',  ( 36.00000000000000711, 34.64101615137755630, 20.00000000000001066 ) ) ;
#5067 = CARTESIAN_POINT ( 'NONE',  ( 4.999999999999999112, 1.676853263447885878, 14.14998813191270166 ) ) ;
#5068 = CIRCLE ( 'NONE', #6464, 0.1000000000000002554 ) ;
#5069 = ORIENTED_EDGE ( 'NONE', *, *, #871, .F. ) ;
#5070 = CARTESIAN_POINT ( 'NONE',  ( 4.999999999999999112, -18.05452603534159195, -9.168210874537770394 ) ) ;
#5071 = DIRECTION ( 'NONE',  ( 0.000000000000000000, 1.000000000000000000, -1.224646799147353207E-16 ) ) ;
#5072 = DIRECTION ( 'NONE',  ( -1.000000000000000000, 0.000000000000000000, -0.000000000000000000 ) ) ;
#5073 = CARTESIAN_POINT ( 'NONE',  ( 0.000000000000000000, 1.676853263447885878, 14.14998813191270166 ) ) ;
#5074 = CIRCLE ( 'NONE', #5885, 9.600000000009600853 ) ;
#5075 = PLANE ( 'NONE',  #5051 ) ;
#5076 = DIRECTION ( 'NONE',  ( 0.000000000000000000, -0.8660254037844432595, 0.4999999999999920619 ) ) ;
#5077 = ORIENTED_EDGE ( 'NONE', *, *, #9470, .T. ) ;
#5078 = ADVANCED_FACE ( 'NONE', ( #3151 ), #4015, .T. ) ;
#5079 = DIRECTION ( 'NONE',  ( -1.000000000000000000, -0.000000000000000000, -0.000000000000000000 ) ) ;
#5080 = FACE_OUTER_BOUND ( 'NONE', #8186, .T. ) ;
#5081 = ORIENTED_EDGE ( 'NONE', *, *, #7927, .F. ) ;
#5082 = CARTESIAN_POINT ( 'NONE',  ( -15.00000000000000000, 40.00000000000000711, 2.149999999999999023 ) ) ;
#5083 = ADVANCED_FACE ( 'NONE', ( #5197 ), #7849, .F. ) ;
#5084 = EDGE_LOOP ( 'NONE', ( #9657, #11921, #6220, #1214 ) ) ;
#5085 = CARTESIAN_POINT ( 'NONE',  ( 36.00000000000000000, 0.000000000000000000, -41.99999999999999289 ) ) ;
#5086 = AXIS2_PLACEMENT_3D ( 'NONE', #12317, #5765, #1087 ) ;
#5087 = CARTESIAN_POINT ( 'NONE',  ( -10.00000000000000000, 0.000000000000000000, 0.000000000000000000 ) ) ;
#5088 = LINE ( 'NONE', #1386, #3560 ) ;
#5089 = FACE_OUTER_BOUND ( 'NONE', #2476, .T. ) ;
#5090 = DIRECTION ( 'NONE',  ( -1.000000000000000000, 0.000000000000000000, -0.000000000000000000 ) ) ;
#5091 = ORIENTED_EDGE ( 'NONE', *, *, #1190, .F. ) ;
#5092 = AXIS2_PLACEMENT_3D ( 'NONE', #10086, #4565, #2449 ) ;
#5093 = ORIENTED_EDGE ( 'NONE', *, *, #4658, .T. ) ;
#5094 = CARTESIAN_POINT ( 'NONE',  ( 42.00000000000000000, 0.000000000000000000, 0.000000000000000000 ) ) ;
#5095 = ADVANCED_FACE ( 'NONE', ( #5328 ), #2376, .T. ) ;
#5096 = ITEM_DEFINED_TRANSFORMATION ( 'NONE', 'NONE', #10044,  #6056 ) ;
#5097 = EDGE_CURVE ( 'NONE', #1854, #9966, #5288, .T. ) ;
#5098 = VERTEX_POINT ( 'NONE', #4315 ) ;
#5099 = EDGE_CURVE ( 'NONE', #9690, #649, #11672, .T. ) ;
#5100 = VECTOR ( 'NONE', #9371, 1000.000000000000000 ) ;
#5101 = DIRECTION ( 'NONE',  ( 0.000000000000000000, 0.000000000000000000, 1.000000000000000000 ) ) ;
#5102 = DIRECTION ( 'NONE',  ( 0.000000000000000000, 0.000000000000000000, 1.000000000000000000 ) ) ;
#5103 = FACE_OUTER_BOUND ( 'NONE', #7406, .T. ) ;
#5104 = FACE_OUTER_BOUND ( 'NONE', #801, .T. ) ;
#5105 = DIRECTION ( 'NONE',  ( 0.000000000000000000, 1.000000000000000000, 3.491481338843133355E-15 ) ) ;
#5106 = ORIENTED_EDGE ( 'NONE', *, *, #5554, .T. ) ;
#5107 = ADVANCED_FACE ( 'NONE', ( #11927 ), #4510, .T. ) ;
#5108 = ORIENTED_EDGE ( 'NONE', *, *, #11189, .F. ) ;
#5109 = SHAPE_REPRESENTATION_RELATIONSHIP ( 'NONE' , 'NONE' ,  #1544, #2564 ) ;
#5110 = EDGE_LOOP ( 'NONE', ( #9545, #11524, #5350, #3131 ) ) ;
#5111 = DIRECTION ( 'NONE',  ( -1.000000000000000000, 0.000000000000000000, 0.000000000000000000 ) ) ;
#5112 = CARTESIAN_POINT ( 'NONE',  ( 0.000000000000000000, 9.168210874537823685, -18.05452603534156353 ) ) ;
#5113 = DIRECTION ( 'NONE',  ( 1.000000000000000000, 0.000000000000000000, -0.000000000000000000 ) ) ;
#5114 = ORIENTED_EDGE ( 'NONE', *, *, #495, .T. ) ;
#5115 = EDGE_CURVE ( 'NONE', #4056, #4830, #5500, .T. ) ;
#5116 = LINE ( 'NONE', #4120, #7969 ) ;
#5117 = CARTESIAN_POINT ( 'NONE',  ( 0.000000000000000000, 21.74405275335766419, -5.984728032764733641 ) ) ;
#5118 = VERTEX_POINT ( 'NONE', #5273 ) ;
#5119 =( NAMED_UNIT ( * ) PLANE_ANGLE_UNIT ( ) SI_UNIT ( $, .RADIAN. ) );
#5120 = DIRECTION ( 'NONE',  ( 1.000000000000000000, 0.000000000000000000, 0.000000000000000000 ) ) ;
#5121 = CARTESIAN_POINT ( 'NONE',  ( 5.200000000000002842, 0.000000000000000000, 2.500000000000000444 ) ) ;
#5122 = ORIENTED_EDGE ( 'NONE', *, *, #5661, .F. ) ;
#5123 = CARTESIAN_POINT ( 'NONE',  ( 45.00000000000000000, -2.941673623582828245, 4.043087470277764162 ) ) ;
#5124 = PRODUCT_DEFINITION_SHAPE ( 'NONE', 'NONE',  #12366 ) ;
#5125 = PLANE ( 'NONE',  #9987 ) ;
#5126 = CARTESIAN_POINT ( 'NONE',  ( 2.499999999999999556, 15.57980286237503620, -22.05152472667113983 ) ) ;
#5127 = CARTESIAN_POINT ( 'NONE',  ( 37.00000000000000711, 3.277848209564065307, -38.49347592122088457 ) ) ;
#5128 = PLANE ( 'NONE',  #3455 ) ;
#5129 = LINE ( 'NONE', #3325, #9047 ) ;
#5130 = ORIENTED_EDGE ( 'NONE', *, *, #2329, .F. ) ;
#5131 = VERTEX_POINT ( 'NONE', #10138 ) ;
#5132 = DIRECTION ( 'NONE',  ( -1.000000000000000000, 0.000000000000000000, 0.000000000000000000 ) ) ;
#5133 = CARTESIAN_POINT ( 'NONE',  ( 34.49784845693389457, 0.000000000000000000, -41.99999999999999289 ) ) ;
#5134 = ORIENTED_EDGE ( 'NONE', *, *, #3270, .T. ) ;
#5135 = DIRECTION ( 'NONE',  ( 1.000000000000000000, -0.000000000000000000, -0.000000000000000000 ) ) ;
#5136 =( REPRESENTATION_RELATIONSHIP ('NONE','NONE', #9709, #8426 ) REPRESENTATION_RELATIONSHIP_WITH_TRANSFORMATION ( #3916 )SHAPE_REPRESENTATION_RELATIONSHIP( ) );
#5137 = ORIENTED_EDGE ( 'NONE', *, *, #7930, .F. ) ;
#5138 = DIRECTION ( 'NONE',  ( 0.000000000000000000, 3.552713678800500140E-15, 1.000000000000000000 ) ) ;
#5139 = EDGE_CURVE ( 'NONE', #1183, #1347, #696, .T. ) ;
#5140 = CYLINDRICAL_SURFACE ( 'NONE', #6003, 9.600000000009600853 ) ;
#5141 = CARTESIAN_POINT ( 'NONE',  ( 25.00000000000000000, 0.000000000000000000, 5.000000000000000000 ) ) ;
#5142 = EDGE_CURVE ( 'NONE', #9147, #432, #699, .T. ) ;
#5143 = FACE_OUTER_BOUND ( 'NONE', #7790, .T. ) ;
#5144 = DIRECTION ( 'NONE',  ( 0.000000000000000000, 0.7071067811865486830, -0.7071067811865463515 ) ) ;
#5145 = ORIENTED_EDGE ( 'NONE', *, *, #2041, .F. ) ;
#5146 = CARTESIAN_POINT ( 'NONE',  ( -26.00000000000000355, 0.000000000000000000, 0.000000000000000000 ) ) ;
#5147 = ORIENTED_EDGE ( 'NONE', *, *, #7689, .T. ) ;
#5148 = CARTESIAN_POINT ( 'NONE',  ( 2.499999999999999556, 15.22291137398922167, 14.46592441914969918 ) ) ;
#5149 = VERTEX_POINT ( 'NONE', #4374 ) ;
#5150 = ADVANCED_FACE ( 'NONE', ( #1565 ), #9208, .T. ) ;
#5151 = LINE ( 'NONE', #9920, #4583 ) ;
#5152 = CIRCLE ( 'NONE', #8969, 8.099999999999999645 ) ;
#5153 = LINE ( 'NONE', #8982, #8591 ) ;
#5154 = CARTESIAN_POINT ( 'NONE',  ( 0.7254551418982898570, 0.5999999999999999778, -3.754038125290899863 ) ) ;
#5155 = EDGE_CURVE ( 'NONE', #3952, #3603, #9298, .T. ) ;
#5156 = AXIS2_PLACEMENT_3D ( 'NONE', #8859, #8786, #8040 ) ;
#5157 = DIRECTION ( 'NONE',  ( 0.000000000000000000, 0.000000000000000000, 1.000000000000000000 ) ) ;
#5159 = ADVANCED_FACE ( 'NONE', ( #8388, #3571, #9095 ), #7390, .F. ) ;
#5158 = LINE ( 'NONE', #7053, #12184 ) ;
#5160 = ORIENTED_EDGE ( 'NONE', *, *, #9838, .T. ) ;
#5161 = DIRECTION ( 'NONE',  ( -1.000000000000000000, -0.000000000000000000, 0.000000000000000000 ) ) ;
#5162 = ORIENTED_EDGE ( 'NONE', *, *, #2972, .T. ) ;
#5163 = DIRECTION ( 'NONE',  ( 0.000000000000000000, 0.000000000000000000, 1.000000000000000000 ) ) ;
#5164 = ORIENTED_EDGE ( 'NONE', *, *, #4168, .F. ) ;
#5166 = CARTESIAN_POINT ( 'NONE',  ( 0.000000000000000000, -17.79862902732275032, 13.85025647830051021 ) ) ;
#5165 = AXIS2_PLACEMENT_3D ( 'NONE', #350, #239, #9933 ) ;
#5167 = AXIS2_PLACEMENT_3D ( 'NONE', #1689, #9381, #12058 ) ;
#5168 = CARTESIAN_POINT ( 'NONE',  ( 36.00000000000000000, 30.00000000000000711, -19.99999999999998934 ) ) ;
#5169 = CARTESIAN_POINT ( 'NONE',  ( 4.999999999999999112, -20.18872947935932061, 1.561154383803151191 ) ) ;
#5170 = PRODUCT_DEFINITION ( 'UNKNOWN', '', #1253, #1379 ) ;
#5171 = VECTOR ( 'NONE', #8157, 1000.000000000000000 ) ;
#5172 = CIRCLE ( 'NONE', #572, 7.500000000000000000 ) ;
#5173 = ORIENTED_EDGE ( 'NONE', *, *, #4957, .F. ) ;
#5174 = AXIS2_PLACEMENT_3D ( 'NONE', #1285, #8923, #1400 ) ;
#5175 = CARTESIAN_POINT ( 'NONE',  ( 0.000000000000000000, 0.000000000000000000, 0.000000000000000000 ) ) ;
#5176 = ORIENTED_EDGE ( 'NONE', *, *, #10799, .F. ) ;
#5177 = DIRECTION ( 'NONE',  ( -1.000000000000000000, -0.000000000000000000, -0.000000000000000000 ) ) ;
#5178 = DIRECTION ( 'NONE',  ( 0.000000000000000000, 0.000000000000000000, 1.000000000000000000 ) ) ;
#5179 = EDGE_LOOP ( 'NONE', ( #3538, #7191, #5649, #2861 ) ) ;
#5180 = CARTESIAN_POINT ( 'NONE',  ( 0.000000000000000000, 8.872489362018390224, -14.40062958310456054 ) ) ;
#5181 = VECTOR ( 'NONE', #10482, 1000.000000000000000 ) ;
#5182 = EDGE_CURVE ( 'NONE', #7570, #12046, #7101, .T. ) ;
#5183 = EDGE_CURVE ( 'NONE', #4573, #2515, #8898, .T. ) ;
#5184 = AXIS2_PLACEMENT_3D ( 'NONE', #3266, #438, #7077 ) ;
#5185 = DIRECTION ( 'NONE',  ( 1.000000000000000000, 0.000000000000000000, 0.000000000000000000 ) ) ;
#5186 = CARTESIAN_POINT ( 'NONE',  ( 65.79898987322334847, -9.445087446769608850E-17, -41.99999999999998579 ) ) ;
#5187 = LINE ( 'NONE', #8086, #10990 ) ;
#5188 = CARTESIAN_POINT ( 'NONE',  ( 0.000000000000000000, 5.984728032764962791, 21.74405275335760379 ) ) ;
#5189 = DIRECTION ( 'NONE',  ( 0.000000000000000000, 0.000000000000000000, 1.000000000000000000 ) ) ;
#5190 = VECTOR ( 'NONE', #7235, 1000.000000000000114 ) ;
#5191 = ORIENTED_EDGE ( 'NONE', *, *, #1326, .T. ) ;
#5192 = VERTEX_POINT ( 'NONE', #7336 ) ;
#5193 = CARTESIAN_POINT ( 'NONE',  ( 4.999999999999999112, 15.57980286237503620, -22.05152472667113628 ) ) ;
#5194 = CARTESIAN_POINT ( 'NONE',  ( 0.000000000000000000, -20.41639017900862996, 4.916402349214513912 ) ) ;
#5195 = AXIS2_PLACEMENT_3D ( 'NONE', #2119, #3813, #6753 ) ;
#5196 = EDGE_LOOP ( 'NONE', ( #9540, #5379, #2688, #7059 ) ) ;
#5197 = FACE_OUTER_BOUND ( 'NONE', #9694, .T. ) ;
#5198 = EDGE_LOOP ( 'NONE', ( #10888, #4261 ) ) ;
#5199 = DIRECTION ( 'NONE',  ( 0.000000000000000000, -9.486769009248163798E-17, 1.000000000000000000 ) ) ;
#5200 =( GEOMETRIC_REPRESENTATION_CONTEXT ( 3 ) GLOBAL_UNCERTAINTY_ASSIGNED_CONTEXT ( ( #5403 ) ) GLOBAL_UNIT_ASSIGNED_CONTEXT ( ( #10028, #10843, #3388 ) ) REPRESENTATION_CONTEXT ( 'NONE', 'WORKASPACE' ) );
#5201 = VECTOR ( 'NONE', #9057, 1000.000000000000000 ) ;
#5202 = DIRECTION ( 'NONE',  ( -1.000000000000000000, 0.000000000000000000, 0.000000000000000000 ) ) ;
#5203 = DIRECTION ( 'NONE',  ( -0.000000000000000000, -0.000000000000000000, 1.000000000000000000 ) ) ;
#5204 = CYLINDRICAL_SURFACE ( 'NONE', #10833, 1.999999999999998224 ) ;
#5205 = DIRECTION ( 'NONE',  ( -1.000000000000000000, 0.000000000000000000, 0.000000000000000000 ) ) ;
#5206 = APPLICATION_CONTEXT ( 'automotive_design' ) ;
#5207 = ORIENTED_EDGE ( 'NONE', *, *, #8592, .F. ) ;
#5208 = DIRECTION ( 'NONE',  ( 0.000000000000000000, -0.4999999999999993894, 0.8660254037844389297 ) ) ;
#5209 = CIRCLE ( 'NONE', #813, 9.600000000009602630 ) ;
#5210 = ORIENTED_EDGE ( 'NONE', *, *, #711, .T. ) ;
#5211 = PLANE ( 'NONE',  #7686 ) ;
#5212 = VECTOR ( 'NONE', #1471, 1000.000000000000000 ) ;
#5213 = AXIS2_PLACEMENT_3D ( 'NONE', #1290, #473, #11899 ) ;
#5214 = VERTEX_POINT ( 'NONE', #12180 ) ;
#5215 = CIRCLE ( 'NONE', #11596, 9.600000000009600853 ) ;
#5216 = VECTOR ( 'NONE', #10411, 1000.000000000000000 ) ;
#5217 = ADVANCED_FACE ( 'NONE', ( #9331 ), #11008, .T. ) ;
#5218 = CARTESIAN_POINT ( 'NONE',  ( 0.000000000000000000, -5.950465759859008053, 20.13931372320386259 ) ) ;
#5219 = PRESENTATION_LAYER_ASSIGNMENT (  '', '', ( #4028 ) ) ;
#5220 = AXIS2_PLACEMENT_3D ( 'NONE', #472, #530, #3300 ) ;
#5221 = AXIS2_PLACEMENT_3D ( 'NONE', #2373, #5326, #10084 ) ;
#5222 = CARTESIAN_POINT ( 'NONE',  ( 2.499999999999999556, -15.57980286237488343, 22.05152472667124997 ) ) ;
#5223 = PLANE ( 'NONE',  #4409 ) ;
#5224 = CIRCLE ( 'NONE', #3627, 5.000000000000000000 ) ;
#5225 = AXIS2_PLACEMENT_3D ( 'NONE', #11646, #8962, #5138 ) ;
#5226 = DIRECTION ( 'NONE',  ( 0.000000000000000000, -0.4999999999999889533, -0.8660254037844451469 ) ) ;
#5227 = DIRECTION ( 'NONE',  ( -1.000000000000000000, 0.000000000000000000, 0.000000000000000000 ) ) ;
#5228 = ORIENTED_EDGE ( 'NONE', *, *, #10824, .T. ) ;
#5229 = LINE ( 'NONE', #9062, #5849 ) ;
#5230 = VERTEX_POINT ( 'NONE', #12000 ) ;
#5231 = ADVANCED_FACE ( 'NONE', ( #9146, #11129, #559 ), #2559, .T. ) ;
#5232 = CARTESIAN_POINT ( 'NONE',  ( 34.50000000000000000, 0.000000000000000000, 0.000000000000000000 ) ) ;
#5233 = ORIENTED_EDGE ( 'NONE', *, *, #8647, .F. ) ;
#5234 = PRESENTATION_LAYER_ASSIGNMENT (  '', '', ( #639 ) ) ;
#5235 = VECTOR ( 'NONE', #9788, 1000.000000000000000 ) ;
#5236 = CARTESIAN_POINT ( 'NONE',  ( 2.500000000000000444, 4.576198416197625463, -26.60936692326685815 ) ) ;
#5237 = AXIS2_PLACEMENT_3D ( 'NONE', #3260, #10924, #9824 ) ;
#5238 = ADVANCED_FACE ( 'NONE', ( #6759 ), #2941, .F. ) ;
#5239 = AXIS2_PLACEMENT_3D ( 'NONE', #5010, #7136, #11692 ) ;
#5240 = DIRECTION ( 'NONE',  ( -1.000000000000000000, 0.000000000000000000, 0.000000000000000000 ) ) ;
#5241 = ADVANCED_FACE ( 'NONE', ( #9460 ), #9646, .F. ) ;
#5242 = EDGE_LOOP ( 'NONE', ( #3275, #8405, #11043, #5061, #4850, #322 ) ) ;
#5243 = CARTESIAN_POINT ( 'NONE',  ( 36.00000000000000000, 0.000000000000000000, -44.50000000000000000 ) ) ;
#5244 = AXIS2_PLACEMENT_3D ( 'NONE', #9421, #4671, #2778 ) ;
#5245 = AXIS2_PLACEMENT_3D ( 'NONE', #1389, #1467, #6211 ) ;
#5246 = AXIS2_PLACEMENT_3D ( 'NONE', #4408, #5161, #1408 ) ;
#5247 = VERTEX_POINT ( 'NONE', #10504 ) ;
#5248 = VECTOR ( 'NONE', #1068, 1000.000000000000000 ) ;
#5249 = DIRECTION ( 'NONE',  ( 1.000000000000000000, 0.000000000000000000, 0.000000000000000000 ) ) ;
#5250 = ORIENTED_EDGE ( 'NONE', *, *, #2581, .F. ) ;
#5251 = CARTESIAN_POINT ( 'NONE',  ( 4.999999999999999112, 15.57980286237472889, 22.05152472667134944 ) ) ;
#5252 = CYLINDRICAL_SURFACE ( 'NONE', #1302, 2.500000000000000444 ) ;
#5253 = EDGE_CURVE ( 'NONE', #922, #9384, #880, .T. ) ;
#5255 = ORIENTED_EDGE ( 'NONE', *, *, #7237, .T. ) ;
#5254 = EDGE_CURVE ( 'NONE', #1609, #8601, #7573, .T. ) ;
#5256 = PLANE ( 'NONE',  #10547 ) ;
#5257 = CIRCLE ( 'NONE', #5862, 40.00000000000000711 ) ;
#5258 = EDGE_CURVE ( 'NONE', #6501, #11122, #1889, .T. ) ;
#5259 = CIRCLE ( 'NONE', #6868, 20.24900000002024569 ) ;
#5260 = CYLINDRICAL_SURFACE ( 'NONE', #2000, 8.099999999999999645 ) ;
#5261 = CYLINDRICAL_SURFACE ( 'NONE', #4199, 7.200000000007202416 ) ;
#5262 = CARTESIAN_POINT ( 'NONE',  ( -0.2500000000000000000, -8.096141056083446585, -1.000000000000000000 ) ) ;
#5263 = CARTESIAN_POINT ( 'NONE',  ( 2.500000000000000444, -14.41081992069293349, -22.83261415639518432 ) ) ;
#5264 = VERTEX_POINT ( 'NONE', #1946 ) ;
#5265 = EDGE_LOOP ( 'NONE', ( #11591, #8959, #69, #5106 ) ) ;
#5266 = CARTESIAN_POINT ( 'NONE',  ( 0.000000000000000000, 0.000000000000000000, 0.000000000000000000 ) ) ;
#5267 = EDGE_CURVE ( 'NONE', #1899, #11027, #1072, .T. ) ;
#5268 = AXIS2_PLACEMENT_3D ( 'NONE', #7512, #998, #3695 ) ;
#5269 = DIRECTION ( 'NONE',  ( 0.000000000000000000, 0.000000000000000000, 1.000000000000000000 ) ) ;
#5270 = DIRECTION ( 'NONE',  ( 0.000000000000000000, 0.000000000000000000, -1.000000000000000000 ) ) ;
#5271 = EDGE_CURVE ( 'NONE', #6734, #2662, #1096, .T. ) ;
#5272 = ORIENTED_EDGE ( 'NONE', *, *, #8852, .T. ) ;
#5273 = CARTESIAN_POINT ( 'NONE',  ( 0.000000000000000000, -1.676853263447986242, 14.14998813191269100 ) ) ;
#5274 = ORIENTED_EDGE ( 'NONE', *, *, #4563, .F. ) ;
#5275 = CYLINDRICAL_SURFACE ( 'NONE', #7239, 27.00000000002699707 ) ;
#5276 = AXIS2_PLACEMENT_3D ( 'NONE', #3727, #5668, #8543 ) ;
#5277 = VERTEX_POINT ( 'NONE', #9388 ) ;
#5278 = DIRECTION ( 'NONE',  ( 0.000000000000000000, 0.000000000000000000, -1.000000000000000000 ) ) ;
#5279 = DIRECTION ( 'NONE',  ( -4.000869187770762975E-18, -0.8386705679454229401, -0.5446390350150287496 ) ) ;
#5280 = CARTESIAN_POINT ( 'NONE',  ( 4.999999999999999112, 5.984728032764962791, 21.74405275335760379 ) ) ;
#5281 = ORIENTED_EDGE ( 'NONE', *, *, #2517, .F. ) ;
#5282 = DIRECTION ( 'NONE',  ( -1.000000000000000000, 0.000000000000000000, 0.000000000000000000 ) ) ;
#5283 = ADVANCED_FACE ( 'NONE', ( #6710 ), #9570, .T. ) ;
#5284 = CARTESIAN_POINT ( 'NONE',  ( -33.00000000000000000, 0.000000000000000000, 0.000000000000000000 ) ) ;
#5285 = ORIENTED_EDGE ( 'NONE', *, *, #11177, .T. ) ;
#5286 = DIRECTION ( 'NONE',  ( 0.000000000000000000, 0.8772744497699203059, 0.4799891038147465760 ) ) ;
#5287 = CONTEXT_DEPENDENT_SHAPE_REPRESENTATION ( #6026, #643 ) ;
#5288 = CIRCLE ( 'NONE', #6098, 5.999999999999999112 ) ;
#5289 = EDGE_LOOP ( 'NONE', ( #6984, #10533, #5337, #5565 ) ) ;
#5290 = LINE ( 'NONE', #9294, #3185 ) ;
#5291 = CARTESIAN_POINT ( 'NONE',  ( 0.000000000000000000, -15.57980286237457257, -22.05152472667146668 ) ) ;
#5292 = CARTESIAN_POINT ( 'NONE',  ( 65.79898987322334847, -9.445087446769608850E-17, -41.99999999999998579 ) ) ;
#5293 = VECTOR ( 'NONE', #7646, 999.9999999999998863 ) ;
#5294 = LINE ( 'NONE', #7052, #5613 ) ;
#5295 = CARTESIAN_POINT ( 'NONE',  ( -3.469446951953614189E-15, 66.91287847477919115, -12.50000000000000000 ) ) ;
#5296 = VERTEX_POINT ( 'NONE', #1818 ) ;
#5297 = DIRECTION ( 'NONE',  ( 0.000000000000000000, -1.000000000000000000, 0.000000000000000000 ) ) ;
#5298 = ORIENTED_EDGE ( 'NONE', *, *, #5785, .F. ) ;
#5299 = CARTESIAN_POINT ( 'NONE',  ( 36.00000000000000711, 1.456773409934505593E-31, -41.99999999999998579 ) ) ;
#5300 = EDGE_LOOP ( 'NONE', ( #9607, #9219 ) ) ;
#5301 = CARTESIAN_POINT ( 'NONE',  ( -0.1481481481481481122, -4.797713218419819903, -1.000000000000000000 ) ) ;
#5302 = AXIS2_PLACEMENT_3D ( 'NONE', #10548, #734, #4549 ) ;
#5303 = CARTESIAN_POINT ( 'NONE',  ( 37.00000000000000711, -3.756272583685665190, -38.69993692832219523 ) ) ;
#5304 = ORIENTED_EDGE ( 'NONE', *, *, #11251, .T. ) ;
#5305 = CARTESIAN_POINT ( 'NONE',  ( 1.399999999999998579, 0.000000000000000000, -7.500000000000000000 ) ) ;
#5306 = EDGE_CURVE ( 'NONE', #9414, #2515, #5824, .T. ) ;
#5307 = EDGE_CURVE ( 'NONE', #1069, #5359, #4884, .T. ) ;
#5308 = ORIENTED_EDGE ( 'NONE', *, *, #3163, .T. ) ;
#5309 = CYLINDRICAL_SURFACE ( 'NONE', #4362, 2.396904916527699214 ) ;
#5310 = VERTEX_POINT ( 'NONE', #4695 ) ;
#5311 = FACE_OUTER_BOUND ( 'NONE', #1599, .T. ) ;
#5312 = ORIENTED_EDGE ( 'NONE', *, *, #4118, .T. ) ;
#5313 = CARTESIAN_POINT ( 'NONE',  ( -3.098410542199071749, -7.060458129626440815, -1.000000000000000000 ) ) ;
#5314 = PLANE ( 'NONE',  #10180 ) ;
#5315 = EDGE_CURVE ( 'NONE', #451, #11627, #10685, .T. ) ;
#5316 = CARTESIAN_POINT ( 'NONE',  ( 0.000000000000000000, 0.5999999999999998668, 2.622672778259560467 ) ) ;
#5317 = LINE ( 'NONE', #6618, #5604 ) ;
#5318 = EDGE_CURVE ( 'NONE', #908, #1305, #898, .T. ) ;
#5319 = ADVANCED_FACE ( 'NONE', ( #11255 ), #8515, .T. ) ;
#5320 = DIRECTION ( 'NONE',  ( 0.000000000000000000, 0.000000000000000000, -1.000000000000000000 ) ) ;
#5321 = DIRECTION ( 'NONE',  ( 0.000000000000000000, 0.000000000000000000, 1.000000000000000000 ) ) ;
#5322 = EDGE_CURVE ( 'NONE', #10725, #3878, #3754, .T. ) ;
#5323 = ORIENTED_EDGE ( 'NONE', *, *, #11230, .T. ) ;
#5324 = ORIENTED_EDGE ( 'NONE', *, *, #1572, .F. ) ;
#5325 = CARTESIAN_POINT ( 'NONE',  ( -15.00000000000000000, 30.00000000000000711, -2.000000000000000000 ) ) ;
#5326 = DIRECTION ( 'NONE',  ( -1.000000000000000000, 0.000000000000000000, -0.000000000000000000 ) ) ;
#5327 = ORIENTED_EDGE ( 'NONE', *, *, #11709, .T. ) ;
#5328 = FACE_OUTER_BOUND ( 'NONE', #11154, .T. ) ;
#5329 = EDGE_LOOP ( 'NONE', ( #8779, #6362, #695, #855 ) ) ;
#5330 = CARTESIAN_POINT ( 'NONE',  ( 15.00000000000000355, 40.00000000000000711, -2.149999999999999023 ) ) ;
#5331 = ORIENTED_EDGE ( 'NONE', *, *, #3935, .F. ) ;
#5332 = LINE ( 'NONE', #568, #11573 ) ;
#5333 = FACE_OUTER_BOUND ( 'NONE', #9390, .T. ) ;
#5334 = CARTESIAN_POINT ( 'NONE',  ( 42.00000000000000000, 0.8169585525225424583, -43.25800585191812075 ) ) ;
#5335 = DIRECTION ( 'NONE',  ( -1.000000000000000000, 0.000000000000000000, 0.000000000000000000 ) ) ;
#5336 = PRODUCT_RELATED_PRODUCT_CATEGORY ( 'part', '', ( #12085 ) ) ;
#5337 = ORIENTED_EDGE ( 'NONE', *, *, #148, .T. ) ;
#5338 = DIRECTION ( 'NONE',  ( 0.000000000000000000, 0.000000000000000000, 1.000000000000000000 ) ) ;
#5339 = CARTESIAN_POINT ( 'NONE',  ( -26.00000000000000355, 30.00000000000000711, 20.00000000000001066 ) ) ;
#5340 = EDGE_LOOP ( 'NONE', ( #6681, #1596, #9723, #8183 ) ) ;
#5341 = CONTEXT_DEPENDENT_SHAPE_REPRESENTATION ( #8411, #12013 ) ;
#5342 = VERTEX_POINT ( 'NONE', #73 ) ;
#5343 = EDGE_CURVE ( 'NONE', #9528, #4099, #9493, .T. ) ;
#5344 = CARTESIAN_POINT ( 'NONE',  ( 46.00000000000000000, -3.499999999999998668, -45.49999999999998579 ) ) ;
#5345 = EDGE_CURVE ( 'NONE', #10474, #9620, #10449, .T. ) ;
#5346 = DIRECTION ( 'NONE',  ( 0.000000000000000000, 0.7900737791495477946, 0.6130117645692876316 ) ) ;
#5347 = DIRECTION ( 'NONE',  ( 1.000000000000000000, 0.000000000000000000, 0.000000000000000000 ) ) ;
#5348 = CARTESIAN_POINT ( 'NONE',  ( 0.000000000000000000, -2.791921004064401579, 22.37914155802284100 ) ) ;
#5349 = DIRECTION ( 'NONE',  ( -1.000000000000000000, 0.000000000000000000, 0.000000000000000000 ) ) ;
#5350 = ORIENTED_EDGE ( 'NONE', *, *, #7079, .T. ) ;
#5351 = DIRECTION ( 'NONE',  ( 0.000000000000000000, 0.000000000000000000, 1.000000000000000000 ) ) ;
#5352 = VERTEX_POINT ( 'NONE', #6946 ) ;
#5353 = DIRECTION ( 'NONE',  ( 1.000000000000000000, -4.770489558936235687E-18, 6.855277276495153692E-34 ) ) ;
#5354 = FILL_AREA_STYLE_COLOUR ( '', #1053 ) ;
#5355 = ORIENTED_EDGE ( 'NONE', *, *, #7913, .F. ) ;
#5356 = LINE ( 'NONE', #4290, #9231 ) ;
#5357 = DIRECTION ( 'NONE',  ( -0.000000000000000000, -0.000000000000000000, 1.000000000000000000 ) ) ;
#5358 = CIRCLE ( 'NONE', #12330, 7.500000000000000000 ) ;
#5359 = VERTEX_POINT ( 'NONE', #5121 ) ;
#5360 = DIRECTION ( 'NONE',  ( -1.000000000000000000, 0.000000000000000000, 0.000000000000000000 ) ) ;
#5361 = ORIENTED_EDGE ( 'NONE', *, *, #9449, .T. ) ;
#5362 = DIRECTION ( 'NONE',  ( 1.000000000000000000, 3.903127820947815962E-18, 0.000000000000000000 ) ) ;
#5363 = AXIS2_PLACEMENT_3D ( 'NONE', #10865, #1168, #3989 ) ;
#5364 = ORIENTED_EDGE ( 'NONE', *, *, #1423, .T. ) ;
#5365 = AXIS2_PLACEMENT_3D ( 'NONE', #1303, #354, #4173 ) ;
#5366 =( NAMED_UNIT ( * ) PLANE_ANGLE_UNIT ( ) SI_UNIT ( $, .RADIAN. ) );
#5367 = CIRCLE ( 'NONE', #10348, 20.24900000002024569 ) ;
#5368 = DIRECTION ( 'NONE',  ( -1.000000000000000000, -0.000000000000000000, -0.000000000000000000 ) ) ;
#5369 = ORIENTED_EDGE ( 'NONE', *, *, #1658, .F. ) ;
#5370 = CARTESIAN_POINT ( 'NONE',  ( 46.00000000000000000, 6.123233995736773185E-16, -46.99999999999999289 ) ) ;
#5371 = ADVANCED_FACE ( 'NONE', ( #10812, #7759 ), #8758, .F. ) ;
#5372 = AXIS2_PLACEMENT_3D ( 'NONE', #7344, #8284, #6340 ) ;
#5373 =( REPRESENTATION_RELATIONSHIP ('NONE','NONE', #9709, #1080 ) REPRESENTATION_RELATIONSHIP_WITH_TRANSFORMATION ( #7920 )SHAPE_REPRESENTATION_RELATIONSHIP( ) );
#5374 = AXIS2_PLACEMENT_3D ( 'NONE', #4991, #9818, #10869 ) ;
#5375 = DIRECTION ( 'NONE',  ( -1.000000000000000000, -0.000000000000000000, -0.000000000000000000 ) ) ;
#5376 = DIRECTION ( 'NONE',  ( -1.000000000000000000, 0.000000000000000000, 0.000000000000000000 ) ) ;
#5377 = CARTESIAN_POINT ( 'NONE',  ( 0.000000000000000000, 0.000000000000000000, 0.000000000000000000 ) ) ;
#5378 = FACE_OUTER_BOUND ( 'NONE', #6865, .T. ) ;
#5379 = ORIENTED_EDGE ( 'NONE', *, *, #567, .T. ) ;
#5380 = ORIENTED_EDGE ( 'NONE', *, *, #4713, .F. ) ;
#5381 = CARTESIAN_POINT ( 'NONE',  ( -4.065758146820644093E-17, -0.5999999999999994227, -2.765548208259129837 ) ) ;
#5382 = DIRECTION ( 'NONE',  ( -1.000000000000000000, 0.000000000000000000, 0.000000000000000000 ) ) ;
#5383 = ORIENTED_EDGE ( 'NONE', *, *, #3999, .T. ) ;
#5384 = DIRECTION ( 'NONE',  ( 1.000000000000000000, 1.734723475976807094E-16, 0.000000000000000000 ) ) ;
#5385 = AXIS2_PLACEMENT_3D ( 'NONE', #6007, #6898, #8897 ) ;
#5386 = EDGE_CURVE ( 'NONE', #9862, #997, #2685, .T. ) ;
#5387 = ORIENTED_EDGE ( 'NONE', *, *, #1734, .T. ) ;
#5388 = DIRECTION ( 'NONE',  ( 0.000000000000000000, 0.000000000000000000, -1.000000000000000000 ) ) ;
#5389 = CLOSED_SHELL ( 'NONE', ( #6558, #12045, #791, #11256, #10448, #10562, #1250, #5241, #7307, #2703, #9976, #10751, #3676, #9784, #10912, #9682, #10342, #6532, #8996, #6116, #1047, #3740, #2492, #6135, #3209, #868, #3271, #6245 ) ) ;
#5390 = ADVANCED_FACE ( 'NONE', ( #4178 ), #6896, .T. ) ;
#5391 = EDGE_CURVE ( 'NONE', #10175, #3842, #2127, .T. ) ;
#5392 = CIRCLE ( 'NONE', #4986, 6.975000000000000533 ) ;
#5393 = CARTESIAN_POINT ( 'NONE',  ( 4.999999999999999112, 0.000000000000000000, 0.000000000000000000 ) ) ;
#5394 = FACE_OUTER_BOUND ( 'NONE', #7682, .T. ) ;
#5395 = MECHANICAL_DESIGN_GEOMETRIC_PRESENTATION_REPRESENTATION (  '', ( #4588 ), #3210 ) ;
#5396 = CARTESIAN_POINT ( 'NONE',  ( 0.000000000000000000, -14.40062958310459251, -1.672489362011137404 ) ) ;
#5397 = DIRECTION ( 'NONE',  ( 0.000000000000000000, 0.000000000000000000, -1.000000000000000000 ) ) ;
#5398 = ORIENTED_EDGE ( 'NONE', *, *, #4661, .F. ) ;
#5399 = CYLINDRICAL_SURFACE ( 'NONE', #9177, 5.000000000000004441 ) ;
#5400 = CARTESIAN_POINT ( 'NONE',  ( 0.000000000000000000, 22.05152472667129970, 15.57980286237480350 ) ) ;
#5401 = VERTEX_POINT ( 'NONE', #11686 ) ;
#5402 = DIRECTION ( 'NONE',  ( 0.000000000000000000, 0.000000000000000000, 1.000000000000000000 ) ) ;
#5403 = UNCERTAINTY_MEASURE_WITH_UNIT (LENGTH_MEASURE( 1.000000000000000082E-05 ), #10028, 'distance_accuracy_value', 'NONE');
#5404 = ORIENTED_EDGE ( 'NONE', *, *, #5253, .T. ) ;
#5405 = EDGE_CURVE ( 'NONE', #11219, #353, #9707, .T. ) ;
#5406 = CIRCLE ( 'NONE', #2824, 7.200000000007203305 ) ;
#5407 = VECTOR ( 'NONE', #993, 1000.000000000000114 ) ;
#5408 = EDGE_CURVE ( 'NONE', #5656, #7570, #3261, .T. ) ;
#5409 = FILL_AREA_STYLE ('',( #1587 ) ) ;
#5410 = DIRECTION ( 'NONE',  ( -1.000000000000000000, -0.000000000000000000, 0.000000000000000000 ) ) ;
#5411 = CARTESIAN_POINT ( 'NONE',  ( 5.000000000000000888, 4.250000000000000000, 0.000000000000000000 ) ) ;
#5412 = DIRECTION ( 'NONE',  ( 0.000000000000000000, 0.000000000000000000, 1.000000000000000000 ) ) ;
#5413 = CARTESIAN_POINT ( 'NONE',  ( 0.000000000000000000, -26.33508479058316709, -5.955107813822780649 ) ) ;
#5414 = VECTOR ( 'NONE', #7012, 1000.000000000000000 ) ;
#5415 = PRODUCT ( 'clamp', 'clamp', '', ( #10409 ) ) ;
#5416 = VERTEX_POINT ( 'NONE', #2248 ) ;
#5417 = CIRCLE ( 'NONE', #1825, 7.500000000000000000 ) ;
#5418 = CARTESIAN_POINT ( 'NONE',  ( 37.00000000000000711, -3.545505594901966262, -38.47446598704267728 ) ) ;
#5419 = AXIS2_PLACEMENT_3D ( 'NONE', #4863, #10674, #11594 ) ;
#5420 = ORIENTED_EDGE ( 'NONE', *, *, #6145, .T. ) ;
#5421 = FACE_OUTER_BOUND ( 'NONE', #3387, .T. ) ;
#5422 = EDGE_CURVE ( 'NONE', #4680, #649, #2074, .T. ) ;
#5424 = EDGE_CURVE ( 'NONE', #6441, #7902, #1127, .T. ) ;
#5423 = VERTEX_POINT ( 'NONE', #10697 ) ;
#5425 = DIRECTION ( 'NONE',  ( 0.000000000000000000, 0.000000000000000000, 1.000000000000000000 ) ) ;
#5426 = CYLINDRICAL_SURFACE ( 'NONE', #11749, 14.24900000001425227 ) ;
#5427 = TOROIDAL_SURFACE ( 'NONE', #7833, 5.100000000000000533, 0.1000000000000001582 ) ;
#5428 = AXIS2_PLACEMENT_3D ( 'NONE', #10147, #1763, #4581 ) ;
#5429 = VERTEX_POINT ( 'NONE', #5946 ) ;
#5430 = CARTESIAN_POINT ( 'NONE',  ( 4.999999999999999112, -15.57980286237457257, -22.05152472667146313 ) ) ;
#5431 = ORIENTED_EDGE ( 'NONE', *, *, #11654, .T. ) ;
#5432 = LINE ( 'NONE', #11976, #9778 ) ;
#5433 = AXIS2_PLACEMENT_3D ( 'NONE', #3777, #4591, #1717 ) ;
#5434 = ORIENTED_EDGE ( 'NONE', *, *, #1572, .T. ) ;
#5435 = AXIS2_PLACEMENT_3D ( 'NONE', #8144, #8906, #11925 ) ;
#5436 = SHAPE_REPRESENTATION_RELATIONSHIP ( 'NONE' , 'NONE' ,  #1080, #6615 ) ;
#5437 = CIRCLE ( 'NONE', #39, 9.600000000009600853 ) ;
#5438 = AXIS2_PLACEMENT_3D ( 'NONE', #8489, #12220, #2671 ) ;
#5439 = DIRECTION ( 'NONE',  ( -1.000000000000000000, 0.000000000000000000, 0.000000000000000000 ) ) ;
#5440 = ORIENTED_EDGE ( 'NONE', *, *, #7706, .F. ) ;
#5441 = LINE ( 'NONE', #6259, #6797 ) ;
#5442 = AXIS2_PLACEMENT_3D ( 'NONE', #7246, #5163, #2346 ) ;
#5443 = CIRCLE ( 'NONE', #10233, 2.000000000000000000 ) ;
#5444 = AXIS2_PLACEMENT_3D ( 'NONE', #5821, #10637, #6829 ) ;
#5445 = CARTESIAN_POINT ( 'NONE',  ( -38.00000000000000000, 7.347880794884118750E-16, 5.999999999999999112 ) ) ;
#5446 = VECTOR ( 'NONE', #2742, 1000.000000000000114 ) ;
#5447 = CARTESIAN_POINT ( 'NONE',  ( 36.00000000000000000, 30.00000000000000711, -19.99999999999998934 ) ) ;
#5448 = DIRECTION ( 'NONE',  ( -1.734723475976807094E-16, 1.000000000000000000, 0.000000000000000000 ) ) ;
#5449 = ORIENTED_EDGE ( 'NONE', *, *, #11194, .T. ) ;
#5450 = ORIENTED_EDGE ( 'NONE', *, *, #4110, .T. ) ;
#5451 = CARTESIAN_POINT ( 'NONE',  ( 0.02377697851851289651, -0.5999999999999995337, -2.905229528491392266 ) ) ;
#5452 = SHAPE_REPRESENTATION_RELATIONSHIP ( 'NONE' , 'NONE' ,  #8907, #4209 ) ;
#5453 = DIRECTION ( 'NONE',  ( 1.000000000000000000, -0.000000000000000000, -0.000000000000000000 ) ) ;
#5454 = AXIS2_PLACEMENT_3D ( 'NONE', #3507, #3691, #688 ) ;
#5455 = VERTEX_POINT ( 'NONE', #9762 ) ;
#5456 = DIRECTION ( 'NONE',  ( 0.000000000000000000, 0.000000000000000000, 1.000000000000000000 ) ) ;
#5457 = AXIS2_PLACEMENT_3D ( 'NONE', #11367, #11439, #10501 ) ;
#5458 = ORIENTED_EDGE ( 'NONE', *, *, #11513, .F. ) ;
#5459 = CYLINDRICAL_SURFACE ( 'NONE', #3435, 4.250000000000000000 ) ;
#5460 = LINE ( 'NONE', #12239, #5248 ) ;
#5461 = CARTESIAN_POINT ( 'NONE',  ( 46.00000000000000000, -3.499999999999998668, -45.49999999999998579 ) ) ;
#5462 = CARTESIAN_POINT ( 'NONE',  ( 36.00000000000000711, 0.000000000000000000, 5.000000000000000000 ) ) ;
#5463 = EDGE_CURVE ( 'NONE', #2486, #5230, #9098, .T. ) ;
#5464 = CIRCLE ( 'NONE', #10852, 6.080745460913608902 ) ;
#5465 = CYLINDRICAL_SURFACE ( 'NONE', #11423, 20.24900000002024569 ) ;
#5466 = DIRECTION ( 'NONE',  ( 0.000000000000000000, 0.000000000000000000, 1.000000000000000000 ) ) ;
#5467 = EDGE_LOOP ( 'NONE', ( #7208, #1438, #4248, #11237 ) ) ;
#5468 = EDGE_CURVE ( 'NONE', #4934, #1870, #9891, .T. ) ;
#5469 = DIRECTION ( 'NONE',  ( 0.000000000000000000, 0.8660254037844398178, -0.4999999999999980571 ) ) ;
#5470 = CARTESIAN_POINT ( 'NONE',  ( 5.200000000000002842, 0.000000000000000000, -2.700000000000000622 ) ) ;
#5471 = ORIENTED_EDGE ( 'NONE', *, *, #78, .T. ) ;
#5472 = DIRECTION ( 'NONE',  ( 1.000000000000000000, 0.000000000000000000, 0.000000000000000000 ) ) ;
#5473 = ORIENTED_EDGE ( 'NONE', *, *, #6020, .F. ) ;
#5474 = AXIS2_PLACEMENT_3D ( 'NONE', #591, #2722, #6539 ) ;
#5475 = FACE_OUTER_BOUND ( 'NONE', #3314, .T. ) ;
#5476 = FACE_OUTER_BOUND ( 'NONE', #5982, .T. ) ;
#5477 = FACE_OUTER_BOUND ( 'NONE', #2003, .T. ) ;
#5478 = EDGE_CURVE ( 'NONE', #4059, #3401, #300, .T. ) ;
#5479 = CARTESIAN_POINT ( 'NONE',  ( 2.499999999999999556, 26.60936692326690789, 4.576198416197345686 ) ) ;
#5480 = CARTESIAN_POINT ( 'NONE',  ( 36.00000000000000711, 7.960204194457796463E-16, -6.500000000000000888 ) ) ;
#5481 = ORIENTED_EDGE ( 'NONE', *, *, #6717, .T. ) ;
#5482 = EDGE_CURVE ( 'NONE', #9771, #3971, #4069, .T. ) ;
#5483 = AXIS2_PLACEMENT_3D ( 'NONE', #10531, #3915, #9488 ) ;
#5484 = EDGE_CURVE ( 'NONE', #11913, #2151, #1249, .T. ) ;
#5485 = CARTESIAN_POINT ( 'NONE',  ( 1.600000000000000089, 0.000000000000000000, 0.000000000000000000 ) ) ;
#5486 = ADVANCED_FACE ( 'NONE', ( #10875 ), #2304, .T. ) ;
#5487 = EDGE_LOOP ( 'NONE', ( #10598, #2443, #5134, #8940, #10100, #3780, #3184, #4710 ) ) ;
#5488 = CARTESIAN_POINT ( 'NONE',  ( 0.000000000000000000, -22.05152472667140984, 15.57980286237465073 ) ) ;
#5489 = APPLICATION_PROTOCOL_DEFINITION ( 'draft international standard', 'automotive_design', 1998, #12232 ) ;
#5490 = ORIENTED_EDGE ( 'NONE', *, *, #2581, .T. ) ;
#5491 = DIRECTION ( 'NONE',  ( 0.03086419753086420623, 0.9995235871707959241, 0.000000000000000000 ) ) ;
#5492 = DIRECTION ( 'NONE',  ( 0.000000000000000000, 0.000000000000000000, -1.000000000000000000 ) ) ;
#5493 = CIRCLE ( 'NONE', #6485, 7.200000000007202416 ) ;
#5494 = ORIENTED_EDGE ( 'NONE', *, *, #4088, .T. ) ;
#5495 = DIRECTION ( 'NONE',  ( -1.000000000000000000, 0.000000000000000000, 0.000000000000000000 ) ) ;
#5496 = EDGE_CURVE ( 'NONE', #6431, #5214, #11481, .T. ) ;
#5497 = ORIENTED_EDGE ( 'NONE', *, *, #6498, .F. ) ;
#5498 = CARTESIAN_POINT ( 'NONE',  ( 4.999999999999999112, -16.90755573046745752, -0.4834863907627537372 ) ) ;
#5499 = ORIENTED_EDGE ( 'NONE', *, *, #5386, .F. ) ;
#5500 = CIRCLE ( 'NONE', #6899, 4.799999999999999822 ) ;
#5501 = DIRECTION ( 'NONE',  ( 0.000000000000000000, 1.224646799147343593E-16, 1.000000000000000000 ) ) ;
#5502 = EDGE_LOOP ( 'NONE', ( #1737, #926, #3046, #1922 ) ) ;
#5503 = DIRECTION ( 'NONE',  ( 0.000000000000000000, 0.000000000000000000, 1.000000000000000000 ) ) ;
#5504 = CARTESIAN_POINT ( 'NONE',  ( 4.999999999999999112, 0.000000000000000000, 0.000000000000000000 ) ) ;
#5505 = ADVANCED_FACE ( 'NONE', ( #1361 ), #9008, .T. ) ;
#5506 = ADVANCED_FACE ( 'NONE', ( #11170 ), #12049, .T. ) ;
#5507 = CYLINDRICAL_SURFACE ( 'NONE', #564, 20.24900000002024569 ) ;
#5508 = DIRECTION ( 'NONE',  ( 0.000000000000000000, -0.8660254037844328234, -0.5000000000000099920 ) ) ;
#5509 = ORIENTED_EDGE ( 'NONE', *, *, #2636, .F. ) ;
#5510 = ORIENTED_EDGE ( 'NONE', *, *, #5182, .F. ) ;
#5511 = CARTESIAN_POINT ( 'NONE',  ( 46.00000000000000000, -3.756272583685664301, -38.69993692832219523 ) ) ;
#5512 = DIRECTION ( 'NONE',  ( 0.000000000000000000, 0.000000000000000000, 1.000000000000000000 ) ) ;
#5513 = DIRECTION ( 'NONE',  ( -1.000000000000000000, -3.903127820947815962E-18, 0.000000000000000000 ) ) ;
#5514 = VERTEX_POINT ( 'NONE', #3501 ) ;
#5515 = DIRECTION ( 'NONE',  ( 0.000000000000000000, -0.5000000000000012212, -0.8660254037844380415 ) ) ;
#5516 = CARTESIAN_POINT ( 'NONE',  ( 0.000000000000000000, -20.18872947935930284, -1.561154383803435408 ) ) ;
#5517 = EDGE_LOOP ( 'NONE', ( #4285, #10634, #10776, #4137 ) ) ;
#5518 = CARTESIAN_POINT ( 'NONE',  ( 4.999999999999999112, -4.916402349214441969, -20.41639017900864772 ) ) ;
#5519 = DIRECTION ( 'NONE',  ( -0.000000000000000000, 1.000000000000000000, -0.000000000000000000 ) ) ;
#5520 = ORIENTED_EDGE ( 'NONE', *, *, #502, .F. ) ;
#5521 = CARTESIAN_POINT ( 'NONE',  ( -25.00000000000000000, 0.000000000000000000, 5.000000000000000000 ) ) ;
#5522 = CARTESIAN_POINT ( 'NONE',  ( 0.000000000000000000, 0.000000000000000000, 2.700000000000000178 ) ) ;
#5523 = ORIENTED_EDGE ( 'NONE', *, *, #6886, .F. ) ;
#5524 = CARTESIAN_POINT ( 'NONE',  ( 4.999999999999999112, 14.40062958310465469, -8.872489362018239234 ) ) ;
#5525 = EDGE_LOOP ( 'NONE', ( #532, #4433, #755, #4359 ) ) ;
#5526 = EDGE_CURVE ( 'NONE', #7918, #451, #7320, .T. ) ;
#5527 = ADVANCED_FACE ( 'NONE', ( #2608, #2542 ), #10123, .F. ) ;
#5528 = DIRECTION ( 'NONE',  ( -1.000000000000000000, 0.000000000000000000, -0.000000000000000000 ) ) ;
#5529 = DIRECTION ( 'NONE',  ( 0.000000000000000000, 0.000000000000000000, 1.000000000000000000 ) ) ;
#5530 = CARTESIAN_POINT ( 'NONE',  ( 20.00000000000000000, 0.000000000000000000, -25.00000000000000000 ) ) ;
#5531 = CYLINDRICAL_SURFACE ( 'NONE', #2834, 6.500000000000000888 ) ;
#5532 = CARTESIAN_POINT ( 'NONE',  ( -20.63749999999999574, 8.541911424052788811E-16, 6.975000000000000533 ) ) ;
#5533 = VERTEX_POINT ( 'NONE', #2360 ) ;
#5534 = ORIENTED_EDGE ( 'NONE', *, *, #4808, .T. ) ;
#5535 = DIRECTION ( 'NONE',  ( 0.000000000000000000, 1.000000000000000000, 0.000000000000000000 ) ) ;
#5536 = EDGE_LOOP ( 'NONE', ( #1012, #1202, #11825, #934 ) ) ;
#5537 = DIRECTION ( 'NONE',  ( -1.000000000000000000, 0.000000000000000000, 0.000000000000000000 ) ) ;
#5538 = PRODUCT_CONTEXT ( 'NONE', #901, 'mechanical' ) ;
#5539 = VERTEX_POINT ( 'NONE', #8262 ) ;
#5540 = CARTESIAN_POINT ( 'NONE',  ( 4.999999999999999112, -8.872489362018288972, 14.40062958310462271 ) ) ;
#5541 = ADVANCED_FACE ( 'NONE', ( #1436 ), #9904, .T. ) ;
#5542 = CARTESIAN_POINT ( 'NONE',  ( -36.00000000000000000, 30.00000000000000711, 20.00000000000001066 ) ) ;
#5543 = EDGE_CURVE ( 'NONE', #6125, #3907, #9701, .T. ) ;
#5544 = EDGE_CURVE ( 'NONE', #3713, #7451, #2498, .T. ) ;
#5545 = ORIENTED_EDGE ( 'NONE', *, *, #10306, .F. ) ;
#5546 = DIRECTION ( 'NONE',  ( -1.000000000000000000, 0.000000000000000000, 0.000000000000000000 ) ) ;
#5547 = FACE_OUTER_BOUND ( 'NONE', #82, .T. ) ;
#5548 = EDGE_LOOP ( 'NONE', ( #8795, #6483 ) ) ;
#5549 = LINE ( 'NONE', #8363, #2985 ) ;
#5550 = ORIENTED_EDGE ( 'NONE', *, *, #4629, .F. ) ;
#5551 = FACE_OUTER_BOUND ( 'NONE', #5611, .T. ) ;
#5552 = ORIENTED_EDGE ( 'NONE', *, *, #2433, .T. ) ;
#5553 = CARTESIAN_POINT ( 'NONE',  ( 4.999999999999999112, -19.24938187143291657, -6.283573709965514453 ) ) ;
#5554 = EDGE_CURVE ( 'NONE', #8041, #9710, #6305, .T. ) ;
#5555 = CARTESIAN_POINT ( 'NONE',  ( 1.250000000000000000, -6.429618962271402616, 0.000000000000000000 ) ) ;
#5556 = CIRCLE ( 'NONE', #1568, 14.24900000001425049 ) ;
#5557 = AXIS2_PLACEMENT_3D ( 'NONE', #1774, #6671, #5851 ) ;
#5558 = CARTESIAN_POINT ( 'NONE',  ( 2.500000000000000000, 2.500728763858895382E-16, -2.041999999999999815 ) ) ;
#5559 = ORIENTED_EDGE ( 'NONE', *, *, #2090, .F. ) ;
#5560 = ORIENTED_EDGE ( 'NONE', *, *, #6727, .F. ) ;
#5561 = DIRECTION ( 'NONE',  ( -1.000000000000000000, 0.000000000000000000, 0.000000000000000000 ) ) ;
#5562 = CARTESIAN_POINT ( 'NONE',  ( 2.499999999999999556, -26.33508479058324880, 5.955107813822412943 ) ) ;
#5563 = CARTESIAN_POINT ( 'NONE',  ( 45.00000000000000000, -3.185523555419108810, 3.853886308373663638 ) ) ;
#5564 = ADVANCED_FACE ( 'NONE', ( #11979 ), #10176, .T. ) ;
#5565 = ORIENTED_EDGE ( 'NONE', *, *, #6088, .T. ) ;
#5566 = FACE_OUTER_BOUND ( 'NONE', #9905, .T. ) ;
#5567 = ADVANCED_FACE ( 'NONE', ( #11059 ), #2429, .F. ) ;
#5568 = AXIS2_PLACEMENT_3D ( 'NONE', #10096, #12015, #4462 ) ;
#5569 = AXIS2_PLACEMENT_3D ( 'NONE', #4932, #4879, #67 ) ;
#5570 = CARTESIAN_POINT ( 'NONE',  ( 4.999999999999997335, 4.769696007084728073, -1.500000000000000000 ) ) ;
#5571 = DIRECTION ( 'NONE',  ( 0.000000000000000000, 0.000000000000000000, 1.000000000000000000 ) ) ;
#5572 = ORIENTED_EDGE ( 'NONE', *, *, #5768, .T. ) ;
#5573 = CARTESIAN_POINT ( 'NONE',  ( 0.000000000000000000, 0.000000000000000000, 0.000000000000000000 ) ) ;
#5574 = CARTESIAN_POINT ( 'NONE',  ( 0.000000000000000000, -11.41582255376079047, 8.527191590521034925 ) ) ;
#5575 = CIRCLE ( 'NONE', #10364, 9.600000000009600853 ) ;
#5576 = CIRCLE ( 'NONE', #7183, 2.700000000000000178 ) ;
#5577 = ORIENTED_EDGE ( 'NONE', *, *, #6629, .F. ) ;
#5578 = CARTESIAN_POINT ( 'NONE',  ( 50.00005079999999680, 0.000000000000000000, 0.000000000000000000 ) ) ;
#5579 = LINE ( 'NONE', #827, #8418 ) ;
#5580 = CIRCLE ( 'NONE', #1791, 5.750000000000000000 ) ;
#5581 = VERTEX_POINT ( 'NONE', #682 ) ;
#5582 = FACE_OUTER_BOUND ( 'NONE', #8126, .T. ) ;
#5583 = ORIENTED_EDGE ( 'NONE', *, *, #3270, .F. ) ;
#5584 = AXIS2_PLACEMENT_3D ( 'NONE', #7050, #2286, #528 ) ;
#5585 = FACE_OUTER_BOUND ( 'NONE', #94, .T. ) ;
#5586 = AXIS2_PLACEMENT_3D ( 'NONE', #8317, #5620, #8507 ) ;
#5587 = DIRECTION ( 'NONE',  ( 0.000000000000000000, 0.000000000000000000, 1.000000000000000000 ) ) ;
#5588 = DIRECTION ( 'NONE',  ( -1.000000000000000000, 0.000000000000000000, 0.000000000000000000 ) ) ;
#5589 = CARTESIAN_POINT ( 'NONE',  ( 33.00000000000000000, 9.184850993605149917E-16, 7.500000000000000888 ) ) ;
#5590 = LINE ( 'NONE', #9412, #12199 ) ;
#5591 = ORIENTED_EDGE ( 'NONE', *, *, #108, .F. ) ;
#5592 = ORIENTED_EDGE ( 'NONE', *, *, #8367, .T. ) ;
#5593 = DIRECTION ( 'NONE',  ( -1.000000000000000000, -0.000000000000000000, -0.000000000000000000 ) ) ;
#5594 = CIRCLE ( 'NONE', #4805, 2.000000000000000000 ) ;
#5595 = EDGE_LOOP ( 'NONE', ( #6751, #7590, #8283, #1753 ) ) ;
#5596 = DIRECTION ( 'NONE',  ( 0.000000000000000000, 0.000000000000000000, 1.000000000000000000 ) ) ;
#5597 = ORIENTED_EDGE ( 'NONE', *, *, #11905, .F. ) ;
#5598 = VECTOR ( 'NONE', #4677, 1000.000000000000000 ) ;
#5599 = FACE_OUTER_BOUND ( 'NONE', #7433, .T. ) ;
#5600 = FACE_OUTER_BOUND ( 'NONE', #11806, .T. ) ;
#5601 = ORIENTED_EDGE ( 'NONE', *, *, #3356, .T. ) ;
#5602 = ORIENTED_EDGE ( 'NONE', *, *, #10614, .T. ) ;
#5603 = DIRECTION ( 'NONE',  ( 0.000000000000000000, 0.000000000000000000, 1.000000000000000000 ) ) ;
#5604 = VECTOR ( 'NONE', #7551, 1000.000000000000000 ) ;
#5605 = VECTOR ( 'NONE', #1984, 1000.000000000000000 ) ;
#5606 = DIRECTION ( 'NONE',  ( 0.000000000000000000, 0.000000000000000000, -1.000000000000000000 ) ) ;
#5607 = DIRECTION ( 'NONE',  ( 0.000000000000000000, 0.000000000000000000, 1.000000000000000000 ) ) ;
#5608 = ADVANCED_FACE ( 'NONE', ( #5311 ), #9130, .T. ) ;
#5609 = ORIENTED_EDGE ( 'NONE', *, *, #7312, .F. ) ;
#5610 = CARTESIAN_POINT ( 'NONE',  ( 50.00005079999999680, 6.799999999999999822, -1.500000000000000000 ) ) ;
#5611 = EDGE_LOOP ( 'NONE', ( #7612, #482, #3293, #7505, #6082, #9127 ) ) ;
#5612 = ADVANCED_FACE ( 'NONE', ( #10001 ), #1549, .F. ) ;
#5613 = VECTOR ( 'NONE', #585, 1000.000000000000000 ) ;
#5614 = CARTESIAN_POINT ( 'NONE',  ( 4.999999999999999112, 18.05452603534165945, 9.168210874537644273 ) ) ;
#5615 = CIRCLE ( 'NONE', #8016, 4.800000000000000711 ) ;
#5616 = CIRCLE ( 'NONE', #8823, 14.24900000001425049 ) ;
#5617 = EDGE_LOOP ( 'NONE', ( #773, #3516, #8775, #11892, #3682, #1212 ) ) ;
#5618 = DIRECTION ( 'NONE',  ( 1.000000000000000000, 0.000000000000000000, -0.000000000000000000 ) ) ;
#5619 = AXIS2_PLACEMENT_3D ( 'NONE', #1165, #3244, #10864 ) ;
#5620 = DIRECTION ( 'NONE',  ( -1.000000000000000000, -0.000000000000000000, -0.000000000000000000 ) ) ;
#5621 =( GEOMETRIC_REPRESENTATION_CONTEXT ( 3 ) GLOBAL_UNCERTAINTY_ASSIGNED_CONTEXT ( ( #2521 ) ) GLOBAL_UNIT_ASSIGNED_CONTEXT ( ( #1562, #4446, #12244 ) ) REPRESENTATION_CONTEXT ( 'NONE', 'WORKASPACE' ) );
#5622 = CIRCLE ( 'NONE', #11214, 5.000000000000000000 ) ;
#5623 = CIRCLE ( 'NONE', #7430, 24.99999999999998579 ) ;
#5624 = CIRCLE ( 'NONE', #1841, 27.00000000002699707 ) ;
#5625 = DIRECTION ( 'NONE',  ( 0.000000000000000000, 0.000000000000000000, 1.000000000000000000 ) ) ;
#5626 = CARTESIAN_POINT ( 'NONE',  ( 45.00000000000000000, 6.123233995736765296E-16, -5.000000000000000000 ) ) ;
#5627 = ORIENTED_EDGE ( 'NONE', *, *, #11451, .F. ) ;
#5628 = ORIENTED_EDGE ( 'NONE', *, *, #7693, .F. ) ;
#5629 = CARTESIAN_POINT ( 'NONE',  ( 37.00000000000000711, 6.123233995736773185E-16, -46.99999999999999289 ) ) ;
#5630 = EDGE_CURVE ( 'NONE', #4119, #6360, #4501, .T. ) ;
#5631 = FACE_OUTER_BOUND ( 'NONE', #4881, .T. ) ;
#5632 = EDGE_CURVE ( 'NONE', #8910, #12289, #7313, .T. ) ;
#5633 = ADVANCED_FACE ( 'NONE', ( #4299 ), #5252, .T. ) ;
#5634 = CARTESIAN_POINT ( 'NONE',  ( 0.000000000000000000, 0.000000000000000000, 0.000000000000000000 ) ) ;
#5635 = ORIENTED_EDGE ( 'NONE', *, *, #1743, .F. ) ;
#5636 = CARTESIAN_POINT ( 'NONE',  ( 1.000000000000000000, -0.5999999999999994227, -4.000000000000000000 ) ) ;
#5637 = MECHANICAL_DESIGN_GEOMETRIC_PRESENTATION_REPRESENTATION (  '', ( #3242 ), #2045 ) ;
#5638 = AXIS2_PLACEMENT_3D ( 'NONE', #5573, #9397, #823 ) ;
#5639 = VECTOR ( 'NONE', #7944, 1000.000000000000000 ) ;
#5640 = CIRCLE ( 'NONE', #4838, 27.00000000002699707 ) ;
#5641 = CARTESIAN_POINT ( 'NONE',  ( 27.38165010660258503, 6.519918414551419517, -39.55446041381592437 ) ) ;
#5642 = DIRECTION ( 'NONE',  ( 1.000000000000000000, 0.000000000000000000, 0.000000000000000000 ) ) ;
#5643 = ADVANCED_FACE ( 'NONE', ( #3366 ), #5739, .T. ) ;
#5644 = EDGE_LOOP ( 'NONE', ( #5609, #298, #264, #6578 ) ) ;
#5645 = DIRECTION ( 'NONE',  ( -1.000000000000000000, -0.000000000000000000, 0.000000000000000000 ) ) ;
#5646 = FACE_OUTER_BOUND ( 'NONE', #7474, .T. ) ;
#5647 = CIRCLE ( 'NONE', #3440, 7.200000000007201528 ) ;
#5648 = VECTOR ( 'NONE', #3668, 1000.000000000000000 ) ;
#5649 = ORIENTED_EDGE ( 'NONE', *, *, #5345, .T. ) ;
#5650 = FACE_OUTER_BOUND ( 'NONE', #11569, .T. ) ;
#5651 = VECTOR ( 'NONE', #4503, 1000.000000000000000 ) ;
#5652 = DIRECTION ( 'NONE',  ( 0.000000000000000000, -1.000000000000000000, 0.000000000000000000 ) ) ;
#5653 = EDGE_LOOP ( 'NONE', ( #10778, #10884, #7557, #8678 ) ) ;
#5654 = CARTESIAN_POINT ( 'NONE',  ( 0.000000000000000000, 0.000000000000000000, 0.000000000000000000 ) ) ;
#5655 = UNCERTAINTY_MEASURE_WITH_UNIT (LENGTH_MEASURE( 1.000000000000000082E-05 ), #8131, 'distance_accuracy_value', 'NONE');
#5656 = VERTEX_POINT ( 'NONE', #11429 ) ;
#5657 = CIRCLE ( 'NONE', #11442, 0.1000000000000002554 ) ;
#5658 = DIRECTION ( 'NONE',  ( 0.000000000000000000, 0.4999999999999948930, 0.8660254037844414832 ) ) ;
#5659 = CARTESIAN_POINT ( 'NONE',  ( -25.39999999999996305, 0.000000000000000000, 0.000000000000000000 ) ) ;
#5660 = CARTESIAN_POINT ( 'NONE',  ( 0.000000000000000000, -6.283573709965444287, 19.24938187143293788 ) ) ;
#5661 = EDGE_CURVE ( 'NONE', #10710, #7536, #1875, .T. ) ;
#5662 = DIRECTION ( 'NONE',  ( 0.000000000000000000, 0.3826834323650841196, 0.9238795325112890700 ) ) ;
#5663 = DIRECTION ( 'NONE',  ( 1.000000000000000000, -0.000000000000000000, -0.000000000000000000 ) ) ;
#5664 = ORIENTED_EDGE ( 'NONE', *, *, #8242, .F. ) ;
#5665 = VERTEX_POINT ( 'NONE', #3806 ) ;
#5666 = CARTESIAN_POINT ( 'NONE',  ( 4.999999999999999112, 1.561154383803221579, 20.18872947935931705 ) ) ;
#5667 = ORIENTED_EDGE ( 'NONE', *, *, #4988, .T. ) ;
#5668 = DIRECTION ( 'NONE',  ( 1.000000000000000000, 0.000000000000000000, 0.000000000000000000 ) ) ;
#5669 = DIRECTION ( 'NONE',  ( 0.000000000000000000, -1.000000000000000000, 0.000000000000000000 ) ) ;
#5670 = AXIS2_PLACEMENT_3D ( 'NONE', #3539, #4598, #2593 ) ;
#5671 = VERTEX_POINT ( 'NONE', #11242 ) ;
#5672 = CYLINDRICAL_SURFACE ( 'NONE', #9367, 9.600000000009600853 ) ;
#5673 = ORIENTED_EDGE ( 'NONE', *, *, #8547, .T. ) ;
#5674 = VERTEX_POINT ( 'NONE', #4741 ) ;
#5675 = DIRECTION ( 'NONE',  ( 0.000000000000000000, 1.000000000000000000, 0.000000000000000000 ) ) ;
#5676 = CIRCLE ( 'NONE', #11060, 0.2000000000000000944 ) ;
#5677 = DIRECTION ( 'NONE',  ( 0.000000000000000000, 0.000000000000000000, 1.000000000000000000 ) ) ;
#5678 = LINE ( 'NONE', #9498, #9615 ) ;
#5679 = ORIENTED_EDGE ( 'NONE', *, *, #3873, .T. ) ;
#5680 = CARTESIAN_POINT ( 'NONE',  ( 4.999999999999999112, -11.14352537685188338, 19.60720892790249081 ) ) ;
#5681 = ORIENTED_EDGE ( 'NONE', *, *, #11489, .F. ) ;
#5682 = EDGE_LOOP ( 'NONE', ( #10698, #6064, #2228, #1463, #9286 ) ) ;
#5683 = LINE ( 'NONE', #8625, #6105 ) ;
#5684 = AXIS2_PLACEMENT_3D ( 'NONE', #4522, #8340, #3399 ) ;
#5685 = ORIENTED_EDGE ( 'NONE', *, *, #785, .T. ) ;
#5686 = CARTESIAN_POINT ( 'NONE',  ( 0.5590169943749478954, 8.266365894244635319E-16, -6.750000000000000000 ) ) ;
#5687 = ADVANCED_FACE ( 'NONE', ( #11484, #2680 ), #4683, .T. ) ;
#5688 = PLANE ( 'NONE',  #11175 ) ;
#5689 = EDGE_CURVE ( 'NONE', #702, #5429, #10490, .T. ) ;
#5690 = AXIS2_PLACEMENT_3D ( 'NONE', #7894, #8006, #11626 ) ;
#5691 = DIRECTION ( 'NONE',  ( 1.000000000000000000, 0.000000000000000000, 0.000000000000000000 ) ) ;
#5692 = FACE_OUTER_BOUND ( 'NONE', #1391, .T. ) ;
#5693 = ORIENTED_EDGE ( 'NONE', *, *, #687, .T. ) ;
#5694 = ORIENTED_EDGE ( 'NONE', *, *, #2118, .F. ) ;
#5695 = CARTESIAN_POINT ( 'NONE',  ( 4.078421086530217288, -3.990950201428958621, 0.000000000000000000 ) ) ;
#5696 = CARTESIAN_POINT ( 'NONE',  ( -0.1481481481481481122, -4.797713218419819903, -1.000000000000000000 ) ) ;
#5697 = DIRECTION ( 'NONE',  ( 0.000000000000000000, 0.000000000000000000, 1.000000000000000000 ) ) ;
#5698 = ORIENTED_EDGE ( 'NONE', *, *, #4499, .F. ) ;
#5699 = DIRECTION ( 'NONE',  ( 0.000000000000000000, -1.000000000000000000, -9.486769009248163798E-17 ) ) ;
#5700 = EDGE_CURVE ( 'NONE', #7247, #8440, #10431, .T. ) ;
#5701 = EDGE_CURVE ( 'NONE', #11004, #5845, #6503, .T. ) ;
#5702 = EDGE_CURVE ( 'NONE', #2216, #10868, #3743, .T. ) ;
#5703 = FACE_OUTER_BOUND ( 'NONE', #1948, .T. ) ;
#5704 = CYLINDRICAL_SURFACE ( 'NONE', #12076, 7.200000000007202416 ) ;
#5705 = DIRECTION ( 'NONE',  ( 0.000000000000000000, 0.000000000000000000, -1.000000000000000000 ) ) ;
#5706 = CARTESIAN_POINT ( 'NONE',  ( 1.199999999999999956, 0.000000000000000000, 2.690429798716874377 ) ) ;
#5707 = ORIENTED_EDGE ( 'NONE', *, *, #10894, .F. ) ;
#5708 = CARTESIAN_POINT ( 'NONE',  ( -3.098410542199071749, -7.060458129626440815, 0.000000000000000000 ) ) ;
#5709 = DIRECTION ( 'NONE',  ( 1.000000000000000000, -0.000000000000000000, 0.000000000000000000 ) ) ;
#5710 = VERTEX_POINT ( 'NONE', #2875 ) ;
#5711 = DIRECTION ( 'NONE',  ( -1.000000000000000000, 0.000000000000000000, 0.000000000000000000 ) ) ;
#5712 = ORIENTED_EDGE ( 'NONE', *, *, #3192, .T. ) ;
#5713 = CARTESIAN_POINT ( 'NONE',  ( 4.999999999999999112, 14.14998813191269633, -1.676853263447935394 ) ) ;
#5714 = DIRECTION ( 'NONE',  ( -1.000000000000000000, -0.000000000000000000, -0.000000000000000000 ) ) ;
#5715 = DIRECTION ( 'NONE',  ( -1.000000000000000000, -0.000000000000000000, 0.000000000000000000 ) ) ;
#5716 = LINE ( 'NONE', #10587, #4031 ) ;
#5717 = DIRECTION ( 'NONE',  ( -0.000000000000000000, 0.000000000000000000, 1.000000000000000000 ) ) ;
#5718 = PRODUCT ( 'MAS-168', 'MAS-168', '', ( #7757 ) ) ;
#5719 = ORIENTED_EDGE ( 'NONE', *, *, #12127, .F. ) ;
#5720 = VERTEX_POINT ( 'NONE', #8561 ) ;
#5721 = DIRECTION ( 'NONE',  ( 1.000000000000000000, 0.000000000000000000, 0.000000000000000000 ) ) ;
#5722 = EDGE_LOOP ( 'NONE', ( #2278, #11622 ) ) ;
#5723 =( NAMED_UNIT ( * ) SI_UNIT ( $, .STERADIAN. ) SOLID_ANGLE_UNIT ( ) );
#5724 = APPLICATION_PROTOCOL_DEFINITION ( 'draft international standard', 'automotive_design', 1998, #7311 ) ;
#5725 = EDGE_LOOP ( 'NONE', ( #288, #3925, #479, #12264, #10848, #1200 ) ) ;
#5726 = ADVANCED_FACE ( 'NONE', ( #5551 ), #988, .T. ) ;
#5727 = CARTESIAN_POINT ( 'NONE',  ( 4.999999999999999112, 5.984728032765264771, -21.74405275335751853 ) ) ;
#5728 = EDGE_CURVE ( 'NONE', #3700, #5859, #5683, .T. ) ;
#5729 = ORIENTED_EDGE ( 'NONE', *, *, #1629, .F. ) ;
#5730 = ORIENTED_EDGE ( 'NONE', *, *, #3395, .F. ) ;
#5731 = DIRECTION ( 'NONE',  ( 0.000000000000000000, 0.000000000000000000, -1.000000000000000000 ) ) ;
#5732 = CARTESIAN_POINT ( 'NONE',  ( 51.00000000000000000, 3.500000000000001332, -38.49999999999998579 ) ) ;
#5733 = CARTESIAN_POINT ( 'NONE',  ( 51.00000000000000000, -7.000000000000007994, -41.99999999999998579 ) ) ;
#5734 = DIRECTION ( 'NONE',  ( 0.000000000000000000, -0.8660254037844328234, -0.5000000000000098810 ) ) ;
#5735 = EDGE_LOOP ( 'NONE', ( #2519, #4126, #5494, #4475 ) ) ;
#5736 = DIRECTION ( 'NONE',  ( 1.000000000000000000, 0.000000000000000000, 0.000000000000000000 ) ) ;
#5737 = ORIENTED_EDGE ( 'NONE', *, *, #3796, .T. ) ;
#5738 = ORIENTED_EDGE ( 'NONE', *, *, #939, .T. ) ;
#5739 = CYLINDRICAL_SURFACE ( 'NONE', #707, 21.00000000002100009 ) ;
#5740 = ORIENTED_EDGE ( 'NONE', *, *, #6921, .F. ) ;
#5741 = CARTESIAN_POINT ( 'NONE',  ( 51.00000000000000000, 1.444447458290426890E-31, -41.99999999999998579 ) ) ;
#5742 = CARTESIAN_POINT ( 'NONE',  ( 4.999999999999999112, -1.676853263447986242, 14.14998813191269100 ) ) ;
#5743 = CARTESIAN_POINT ( 'NONE',  ( 0.09977878429777278790, -0.6000000000000000888, 3.189823563989766964 ) ) ;
#5744 = CARTESIAN_POINT ( 'NONE',  ( 4.999999999999999112, 5.950465759858867720, 20.13931372320390523 ) ) ;
#5745 = VERTEX_POINT ( 'NONE', #7628 ) ;
#5746 = DIRECTION ( 'NONE',  ( 1.000000000000000000, 0.000000000000000000, 0.000000000000000000 ) ) ;
#5747 = PRESENTATION_STYLE_ASSIGNMENT (( #1944 ) ) ;
#5748 = CARTESIAN_POINT ( 'NONE',  ( 17.00000000000000000, 2.516649172247811061E-16, -2.055000000000000160 ) ) ;
#5749 = CARTESIAN_POINT ( 'NONE',  ( 36.00000000000000711, 0.000000000000000000, 0.000000000000000000 ) ) ;
#5750 = EDGE_CURVE ( 'NONE', #9337, #138, #12233, .T. ) ;
#5751 = ORIENTED_EDGE ( 'NONE', *, *, #1947, .F. ) ;
#5752 = DIRECTION ( 'NONE',  ( 1.000000000000000000, 0.000000000000000000, 0.000000000000000000 ) ) ;
#5753 = AXIS2_PLACEMENT_3D ( 'NONE', #4434, #6317, #11244 ) ;
#5754 = VECTOR ( 'NONE', #9782, 1000.000000000000000 ) ;
#5755 = FILL_AREA_STYLE ('',( #11377 ) ) ;
#5756 = DIRECTION ( 'NONE',  ( 0.000000000000000000, 0.000000000000000000, 1.000000000000000000 ) ) ;
#5757 = LINE ( 'NONE', #80, #3264 ) ;
#5758 = CARTESIAN_POINT ( 'NONE',  ( 2.499999999999999556, 5.955107813822504426, 26.33508479058322749 ) ) ;
#5759 = ORIENTED_EDGE ( 'NONE', *, *, #10968, .T. ) ;
#5760 = EDGE_CURVE ( 'NONE', #10934, #7180, #8439, .T. ) ;
#5761 = CARTESIAN_POINT ( 'NONE',  ( 0.000000000000000000, 5.984728032765264771, -21.74405275335751853 ) ) ;
#5762 = DIRECTION ( 'NONE',  ( 0.000000000000000000, 0.000000000000000000, -1.000000000000000000 ) ) ;
#5763 = AXIS2_PLACEMENT_3D ( 'NONE', #10625, #6884, #10687 ) ;
#5764 = ORIENTED_EDGE ( 'NONE', *, *, #8557, .F. ) ;
#5765 = DIRECTION ( 'NONE',  ( 1.000000000000000000, 0.000000000000000000, 0.000000000000000000 ) ) ;
#5766 = UNCERTAINTY_MEASURE_WITH_UNIT (LENGTH_MEASURE( 1.000000000000000082E-05 ), #3888, 'distance_accuracy_value', 'NONE');
#5767 = CIRCLE ( 'NONE', #9168, 1.999999999999998224 ) ;
#5768 = EDGE_CURVE ( 'NONE', #2515, #9277, #1936, .T. ) ;
#5769 = ORIENTED_EDGE ( 'NONE', *, *, #11051, .F. ) ;
#5770 = EDGE_CURVE ( 'NONE', #317, #11797, #10690, .T. ) ;
#5771 = DIRECTION ( 'NONE',  ( 0.000000000000000000, -1.000000000000000000, 0.000000000000000000 ) ) ;
#5772 = AXIS2_PLACEMENT_3D ( 'NONE', #9221, #7404, #6214 ) ;
#5773 =( REPRESENTATION_RELATIONSHIP ('NONE','NONE', #9709, #11292 ) REPRESENTATION_RELATIONSHIP_WITH_TRANSFORMATION ( #4853 )SHAPE_REPRESENTATION_RELATIONSHIP( ) );
#5774 = CYLINDRICAL_SURFACE ( 'NONE', #4604, 9.600000000009600853 ) ;
#5775 = DIRECTION ( 'NONE',  ( -1.000000000000000000, 0.000000000000000000, -0.000000000000000000 ) ) ;
#5776 = AXIS2_PLACEMENT_3D ( 'NONE', #11057, #2487, #6311 ) ;
#5777=STYLED_ITEM('',(#12412),#259);
#5778 = DIRECTION ( 'NONE',  ( 0.000000000000000000, 0.000000000000000000, 1.000000000000000000 ) ) ;
#5779 = DIRECTION ( 'NONE',  ( -1.000000000000000000, 0.000000000000000000, 0.000000000000000000 ) ) ;
#5780 = ORIENTED_EDGE ( 'NONE', *, *, #11800, .F. ) ;
#5781 = EDGE_LOOP ( 'NONE', ( #8892, #1508, #1487, #7386 ) ) ;
#5782 =( NAMED_UNIT ( * ) PLANE_ANGLE_UNIT ( ) SI_UNIT ( $, .RADIAN. ) );
#5783 = ORIENTED_EDGE ( 'NONE', *, *, #9696, .F. ) ;
#5784 = FACE_OUTER_BOUND ( 'NONE', #8272, .T. ) ;
#5785 = EDGE_CURVE ( 'NONE', #4782, #4594, #12271, .T. ) ;
#5786 = ITEM_DEFINED_TRANSFORMATION ( 'NONE', 'NONE', #11434,  #6056 ) ;
#5787 = EDGE_CURVE ( 'NONE', #3359, #4406, #8825, .T. ) ;
#5788 = ORIENTED_EDGE ( 'NONE', *, *, #1883, .T. ) ;
#5789 = ADVANCED_FACE ( 'NONE', ( #7503, #11300 ), #2735, .F. ) ;
#5790 = CIRCLE ( 'NONE', #6581, 5.000000000000004441 ) ;
#5791 = VECTOR ( 'NONE', #3263, 1000.000000000000000 ) ;
#5792 = PRESENTATION_LAYER_ASSIGNMENT (  '', '', ( #4384 ) ) ;
#5793 = VERTEX_POINT ( 'NONE', #3126 ) ;
#5794 = ORIENTED_EDGE ( 'NONE', *, *, #10509, .F. ) ;
#5795 = CARTESIAN_POINT ( 'NONE',  ( 24.00000000000000000, 7.347880794884122694E-16, -35.99999999999999289 ) ) ;
#5796 = DIRECTION ( 'NONE',  ( -0.000000000000000000, -0.000000000000000000, -1.000000000000000000 ) ) ;
#5797 = CARTESIAN_POINT ( 'NONE',  ( 0.000000000000000000, 0.000000000000000000, 0.000000000000000000 ) ) ;
#5798 = DIRECTION ( 'NONE',  ( 0.000000000000000000, 0.000000000000000000, 1.000000000000000000 ) ) ;
#5799 = VECTOR ( 'NONE', #4589, 999.9999999999998863 ) ;
#5800 = ORIENTED_EDGE ( 'NONE', *, *, #11050, .F. ) ;
#5801 = ADVANCED_FACE ( 'NONE', ( #299 ), #2234, .T. ) ;
#5802 = EDGE_CURVE ( 'NONE', #7451, #3410, #3425, .T. ) ;
#5803 = AXIS2_PLACEMENT_3D ( 'NONE', #5504, #1744, #797 ) ;
#5804 = DIRECTION ( 'NONE',  ( 0.000000000000000000, -6.982962677686267499E-15, 1.000000000000000000 ) ) ;
#5805 = ORIENTED_EDGE ( 'NONE', *, *, #9133, .T. ) ;
#5806 = ORIENTED_EDGE ( 'NONE', *, *, #7106, .T. ) ;
#5807 = LINE ( 'NONE', #9808, #10214 ) ;
#5808 = ORIENTED_EDGE ( 'NONE', *, *, #11489, .T. ) ;
#5809 = CARTESIAN_POINT ( 'NONE',  ( 42.00000000000000000, 5.702959862028875726, -38.29645456189778940 ) ) ;
#5810 = AXIS2_PLACEMENT_3D ( 'NONE', #11812, #3269, #11989 ) ;
#5811 = AXIS2_PLACEMENT_3D ( 'NONE', #2729, #3427, #10169 ) ;
#5812 = LINE ( 'NONE', #11676, #10584 ) ;
#5813 = ADVANCED_FACE ( 'NONE', ( #5881 ), #5988, .T. ) ;
#5814 = CARTESIAN_POINT ( 'NONE',  ( -3.444205370125434777E-14, -0.6000000000000000888, 2.905564161116319877 ) ) ;
#5815 = CARTESIAN_POINT ( 'NONE',  ( 4.999999999999999112, 0.000000000000000000, 0.000000000000000000 ) ) ;
#5816 = PRESENTATION_LAYER_ASSIGNMENT (  '', '', ( #2607 ) ) ;
#5817 = EDGE_LOOP ( 'NONE', ( #4907, #9142 ) ) ;
#5818 = AXIS2_PLACEMENT_3D ( 'NONE', #3655, #1708, #12193 ) ;
#5819 = LINE ( 'NONE', #4935, #1073 ) ;
#5820 = AXIS2_PLACEMENT_3D ( 'NONE', #1718, #11153, #3535 ) ;
#5821 = CARTESIAN_POINT ( 'NONE',  ( 15.00000000000000355, 44.00000000000001421, 0.000000000000000000 ) ) ;
#5822 = VECTOR ( 'NONE', #2711, 1000.000000000000000 ) ;
#5823 = AXIS2_PLACEMENT_3D ( 'NONE', #12336, #6608, #3607 ) ;
#5824 = LINE ( 'NONE', #5563, #8294 ) ;
#5825 = ORIENTED_EDGE ( 'NONE', *, *, #8386, .F. ) ;
#5826 = DIRECTION ( 'NONE',  ( -0.000000000000000000, -0.000000000000000000, -1.000000000000000000 ) ) ;
#5827 = CIRCLE ( 'NONE', #3230, 27.00000000002699707 ) ;
#5828 = VECTOR ( 'NONE', #5453, 1000.000000000000000 ) ;
#5829 = PRODUCT_DEFINITION_SHAPE ( 'NONE', 'NONE',  #9774 ) ;
#5830 = CIRCLE ( 'NONE', #426, 7.500000000000000000 ) ;
#5831 = AXIS2_PLACEMENT_3D ( 'NONE', #1567, #9278, #5388 ) ;
#5832 = CARTESIAN_POINT ( 'NONE',  ( 4.999999999999999112, 14.14998813191269633, 1.676853263447936726 ) ) ;
#5833 = PLANE ( 'NONE',  #11980 ) ;
#5834 = CARTESIAN_POINT ( 'NONE',  ( -36.00000000000000000, 40.00000000000000711, 20.00000000000001066 ) ) ;
#5835 = DIRECTION ( 'NONE',  ( 0.000000000000000000, 0.6828850436591804574, 0.7305258497456468270 ) ) ;
#5836 = ORIENTED_EDGE ( 'NONE', *, *, #804, .F. ) ;
#5837 = CYLINDRICAL_SURFACE ( 'NONE', #3196, 7.200000000007202416 ) ;
#5838 = CYLINDRICAL_SURFACE ( 'NONE', #8037, 2.149999999999999023 ) ;
#5839 = PRESENTATION_LAYER_ASSIGNMENT (  '', '', ( #3242 ) ) ;
#5840 = AXIS2_PLACEMENT_3D ( 'NONE', #5348, #2403, #9170 ) ;
#5841 = ORIENTED_EDGE ( 'NONE', *, *, #2720, .F. ) ;
#5842 = DIRECTION ( 'NONE',  ( 1.000000000000000000, -0.000000000000000000, -0.000000000000000000 ) ) ;
#5843 = CIRCLE ( 'NONE', #8249, 4.250000000000000000 ) ;
#5844 = AXIS2_PLACEMENT_3D ( 'NONE', #3708, #1831, #5835 ) ;
#5845 = VERTEX_POINT ( 'NONE', #7747 ) ;
#5846 = EDGE_CURVE ( 'NONE', #4782, #9862, #5807, .T. ) ;
#5847 = PRODUCT_DEFINITION_FORMATION_WITH_SPECIFIED_SOURCE ( 'ANY', '', #9932, .NOT_KNOWN. ) ;
#5848 = CIRCLE ( 'NONE', #7447, 9.600000000009604406 ) ;
#5849 = VECTOR ( 'NONE', #11849, 1000.000000000000000 ) ;
#5850 = CYLINDRICAL_SURFACE ( 'NONE', #1006, 6.000000000000005329 ) ;
#5851 = DIRECTION ( 'NONE',  ( 0.000000000000000000, 0.8772744497699203059, 0.4799891038147465760 ) ) ;
#5852 = EDGE_CURVE ( 'NONE', #8559, #4349, #1624, .T. ) ;
#5853 = CIRCLE ( 'NONE', #2859, 14.24900000001425049 ) ;
#5854 = CARTESIAN_POINT ( 'NONE',  ( 0.000000000000000000, -2.357898499370432610, 3.252606517456513302E-15 ) ) ;
#5855 = CYLINDRICAL_SURFACE ( 'NONE', #10809, 7.200000000007202416 ) ;
#5856 = ORIENTED_EDGE ( 'NONE', *, *, #6886, .T. ) ;
#5857 = ORIENTED_EDGE ( 'NONE', *, *, #10946, .F. ) ;
#5858 = SURFACE_STYLE_FILL_AREA ( #1213 ) ;
#5859 = VERTEX_POINT ( 'NONE', #8744 ) ;
#5860 = DIRECTION ( 'NONE',  ( 1.000000000000000000, 0.000000000000000000, 0.000000000000000000 ) ) ;
#5861 = EDGE_LOOP ( 'NONE', ( #7668, #8743, #7882, #1523, #10537 ) ) ;
#5862 = AXIS2_PLACEMENT_3D ( 'NONE', #8953, #8901, #315 ) ;
#5863 = AXIS2_PLACEMENT_3D ( 'NONE', #3328, #7140, #8382 ) ;
#5864 =( REPRESENTATION_RELATIONSHIP ('NONE','NONE', #9709, #11292 ) REPRESENTATION_RELATIONSHIP_WITH_TRANSFORMATION ( #5096 )SHAPE_REPRESENTATION_RELATIONSHIP( ) );
#5865 = ADVANCED_FACE ( 'NONE', ( #3068, #9692 ), #10684, .F. ) ;
#5866 = ORIENTED_EDGE ( 'NONE', *, *, #11735, .T. ) ;
#5867 = ORIENTED_EDGE ( 'NONE', *, *, #4874, .T. ) ;
#5868 = CARTESIAN_POINT ( 'NONE',  ( -1.399999999999998579, 0.000000000000000000, 0.000000000000000000 ) ) ;
#5869 = CARTESIAN_POINT ( 'NONE',  ( 0.1481481481481481122, -4.797713218419819903, 0.000000000000000000 ) ) ;
#5870 = EDGE_CURVE ( 'NONE', #2301, #5149, #10793, .T. ) ;
#5871 = ADVANCED_FACE ( 'NONE', ( #3987 ), #8690, .T. ) ;
#5872 = CARTESIAN_POINT ( 'NONE',  ( 2.499999999999998668, -20.41639017900862996, 4.916402349214513912 ) ) ;
#5874 = EDGE_CURVE ( 'NONE', #1234, #3524, #7881, .T. ) ;
#5873 = CARTESIAN_POINT ( 'NONE',  ( 36.00000000000000711, 0.000000000000000000, 0.000000000000000000 ) ) ;
#5875 = EDGE_LOOP ( 'NONE', ( #10517, #1617, #8585, #381 ) ) ;
#5876 = AXIS2_PLACEMENT_3D ( 'NONE', #2939, #9329, #4123 ) ;
#5877 = SHAPE_REPRESENTATION ( 'slotted pan head screw_iso_ISO 1580 - M4 x 12 - 12N', ( #6056 ), #10030 ) ;
#5878 = DIRECTION ( 'NONE',  ( 0.000000000000000000, 1.000000000000000000, 3.614007241614733816E-15 ) ) ;
#5879 = ORIENTED_EDGE ( 'NONE', *, *, #5760, .T. ) ;
#5880 = VERTEX_POINT ( 'NONE', #115 ) ;
#5881 = FACE_OUTER_BOUND ( 'NONE', #6089, .T. ) ;
#5882 = ORIENTED_EDGE ( 'NONE', *, *, #2910, .T. ) ;
#5883 = DIRECTION ( 'NONE',  ( 1.000000000000000000, 0.000000000000000000, 0.000000000000000000 ) ) ;
#5884 = EDGE_CURVE ( 'NONE', #10459, #9911, #5021, .T. ) ;
#5885 = AXIS2_PLACEMENT_3D ( 'NONE', #2098, #5860, #9541 ) ;
#5886 = DIRECTION ( 'NONE',  ( -1.000000000000000000, -0.000000000000000000, -0.000000000000000000 ) ) ;
#5887 = ORIENTED_EDGE ( 'NONE', *, *, #884, .T. ) ;
#5888 = CARTESIAN_POINT ( 'NONE',  ( 0.7245795732250854826, -0.6000000000000001998, 3.753610258581185910 ) ) ;
#5889 = CYLINDRICAL_SURFACE ( 'NONE', #12038, 7.200000000007202416 ) ;
#5890 = ORIENTED_EDGE ( 'NONE', *, *, #5701, .F. ) ;
#5891 = FACE_OUTER_BOUND ( 'NONE', #10325, .T. ) ;
#5892 = AXIS2_PLACEMENT_3D ( 'NONE', #3281, #4194, #6908 ) ;
#5893 = CARTESIAN_POINT ( 'NONE',  ( 25.00000000000000000, 0.000000000000000000, 0.000000000000000000 ) ) ;
#5894 = DIRECTION ( 'NONE',  ( 0.000000000000000000, 1.000000000000000000, 3.491481338843133750E-15 ) ) ;
#5895 = ORIENTED_EDGE ( 'NONE', *, *, #8013, .F. ) ;
#5896 = DIRECTION ( 'NONE',  ( 0.000000000000000000, 0.000000000000000000, -1.000000000000000000 ) ) ;
#5897 = ADVANCED_FACE ( 'NONE', ( #11671 ), #11607, .T. ) ;
#5898 = ADVANCED_FACE ( 'NONE', ( #7934 ), #6882, .T. ) ;
#5899 = AXIS2_PLACEMENT_3D ( 'NONE', #12304, #3823, #2692 ) ;
#5900 = CARTESIAN_POINT ( 'NONE',  ( 36.00000000000000711, 12.50000000000000000, -24.50000000000000000 ) ) ;
#5901 = CARTESIAN_POINT ( 'NONE',  ( 4.999999999999999112, -11.41582255376066968, -8.527191590521194797 ) ) ;
#5902 = CARTESIAN_POINT ( 'NONE',  ( 43.00000000000000000, -3.792354139917828881, -2.942456469932581253 ) ) ;
#5903 = CARTESIAN_POINT ( 'NONE',  ( 0.000000000000000000, -22.37914155802283034, -2.791921004064479739 ) ) ;
#5904 = EDGE_LOOP ( 'NONE', ( #9357, #374, #5601, #10150 ) ) ;
#5905 = CARTESIAN_POINT ( 'NONE',  ( 4.999999999999999112, 0.000000000000000000, 0.000000000000000000 ) ) ;
#5906 = CYLINDRICAL_SURFACE ( 'NONE', #10604, 14.24900000001425227 ) ;
#5907 = ORIENTED_EDGE ( 'NONE', *, *, #8827, .F. ) ;
#5908 = DIRECTION ( 'NONE',  ( -1.000000000000000000, -0.000000000000000000, -0.000000000000000000 ) ) ;
#5909 = AXIS2_PLACEMENT_3D ( 'NONE', #11861, #5368, #6365 ) ;
#5910 = ORIENTED_EDGE ( 'NONE', *, *, #125, .T. ) ;
#5911 = DIRECTION ( 'NONE',  ( 1.000000000000000000, 0.000000000000000000, 0.000000000000000000 ) ) ;
#5912 = DIRECTION ( 'NONE',  ( -1.000000000000000000, -0.000000000000000000, -0.000000000000000000 ) ) ;
#5913 = CARTESIAN_POINT ( 'NONE',  ( 0.000000000000000000, 0.000000000000000000, 0.000000000000000000 ) ) ;
#5914 = CARTESIAN_POINT ( 'NONE',  ( 4.999999999999999112, 9.168210874537576771, 18.05452603534168432 ) ) ;
#5915 = CARTESIAN_POINT ( 'NONE',  ( 29.56763832957518545, 0.000000000000000000, 1.500000000000000000 ) ) ;
#5916 = ORIENTED_EDGE ( 'NONE', *, *, #147, .T. ) ;
#5917 = VERTEX_POINT ( 'NONE', #348 ) ;
#5918 = CARTESIAN_POINT ( 'NONE',  ( 2.500000000000000000, -1.178949249685213863, 2.042000000000002924 ) ) ;
#5919 = APPLICATION_PROTOCOL_DEFINITION ( 'draft international standard', 'automotive_design', 1998, #7938 ) ;
#5920 = ORIENTED_EDGE ( 'NONE', *, *, #7865, .T. ) ;
#5921 = ADVANCED_FACE ( 'NONE', ( #10620 ), #6932, .T. ) ;
#5922 = DIRECTION ( 'NONE',  ( -1.000000000000000000, -0.000000000000000000, -0.000000000000000000 ) ) ;
#5923 = VERTEX_POINT ( 'NONE', #2164 ) ;
#5924 = DIRECTION ( 'NONE',  ( 0.000000000000000000, 0.7512545167371323940, -0.6600126143355576902 ) ) ;
#5925 = CARTESIAN_POINT ( 'NONE',  ( 4.999999999999999112, 13.17168466712950092, -15.37949036966198157 ) ) ;
#5926 = DIRECTION ( 'NONE',  ( 0.000000000000000000, 0.000000000000000000, -1.000000000000000000 ) ) ;
#5927 = DIRECTION ( 'NONE',  ( -1.000000000000000000, 0.000000000000000000, 0.000000000000000000 ) ) ;
#5928 = ORIENTED_EDGE ( 'NONE', *, *, #8460, .T. ) ;
#5929 = VERTEX_POINT ( 'NONE', #5933 ) ;
#5930 = EDGE_CURVE ( 'NONE', #3666, #733, #9418, .T. ) ;
#5931 = FILL_AREA_STYLE_COLOUR ( '', #4641 ) ;
#5932 = ORIENTED_EDGE ( 'NONE', *, *, #2402, .F. ) ;
#5933 = CARTESIAN_POINT ( 'NONE',  ( 36.00000000000000000, 34.64101615137755630, 20.00000000000001066 ) ) ;
#5934 = EDGE_CURVE ( 'NONE', #8451, #486, #10113, .T. ) ;
#5935 = ORIENTED_EDGE ( 'NONE', *, *, #6164, .T. ) ;
#5936 = DIRECTION ( 'NONE',  ( -1.000000000000000000, 0.000000000000000000, 0.000000000000000000 ) ) ;
#5937 = EDGE_CURVE ( 'NONE', #8121, #4854, #2413, .T. ) ;
#5938 = CYLINDRICAL_SURFACE ( 'NONE', #6807, 40.00000000000000711 ) ;
#5939 = ORIENTED_EDGE ( 'NONE', *, *, #5258, .F. ) ;
#5940 = DIRECTION ( 'NONE',  ( -1.000000000000000000, -0.000000000000000000, -0.000000000000000000 ) ) ;
#5941 = DIRECTION ( 'NONE',  ( -1.000000000000000000, -0.000000000000000000, 0.000000000000000000 ) ) ;
#5942 = ORIENTED_EDGE ( 'NONE', *, *, #749, .F. ) ;
#5943 = LINE ( 'NONE', #3188, #7073 ) ;
#5944 = SURFACE_SIDE_STYLE ('',( #9005 ) ) ;
#5945 = DIRECTION ( 'NONE',  ( -0.7071067811865369146, 8.659560562355062281E-17, -0.7071067811865582309 ) ) ;
#5946 = CARTESIAN_POINT ( 'NONE',  ( 1.400000000000001910, 0.000000000000000000, -5.000000000000000000 ) ) ;
#5947 = ORIENTED_EDGE ( 'NONE', *, *, #12009, .T. ) ;
#5948 = DIRECTION ( 'NONE',  ( 0.000000000000000000, 0.000000000000000000, -1.000000000000000000 ) ) ;
#5949 = EDGE_CURVE ( 'NONE', #718, #4119, #8227, .T. ) ;
#5950 = CARTESIAN_POINT ( 'NONE',  ( 45.00000000000000000, 4.769696007084727185, -1.500000000000000000 ) ) ;
#5951 = DIRECTION ( 'NONE',  ( -1.000000000000000000, 0.000000000000000000, 0.000000000000000000 ) ) ;
#5952 = DIRECTION ( 'NONE',  ( -1.000000000000000000, -0.000000000000000000, -0.000000000000000000 ) ) ;
#5953 = PLANE ( 'NONE',  #1444 ) ;
#5954 = ORIENTED_EDGE ( 'NONE', *, *, #5496, .T. ) ;
#5955 = FACE_OUTER_BOUND ( 'NONE', #8095, .T. ) ;
#5956 = EDGE_CURVE ( 'NONE', #504, #4854, #6634, .T. ) ;
#5957 = DIRECTION ( 'NONE',  ( -0.000000000000000000, -0.000000000000000000, -1.000000000000000000 ) ) ;
#5958 = ADVANCED_FACE ( 'NONE', ( #2348 ), #3307, .T. ) ;
#5959 = ORIENTED_EDGE ( 'NONE', *, *, #11866, .T. ) ;
#5960 = CARTESIAN_POINT ( 'NONE',  ( 16.55500000000001393, 0.000000000000000000, 0.000000000000000000 ) ) ;
#5961 = ORIENTED_EDGE ( 'NONE', *, *, #3515, .T. ) ;
#5962 = DIRECTION ( 'NONE',  ( 1.000000000000000000, -0.000000000000000000, -0.000000000000000000 ) ) ;
#5963 = DIRECTION ( 'NONE',  ( 0.000000000000000000, 0.000000000000000000, 1.000000000000000000 ) ) ;
#5964 = CARTESIAN_POINT ( 'NONE',  ( 4.999999999999999112, 18.05452603534179090, -9.168210874537381372 ) ) ;
#5965 = DIRECTION ( 'NONE',  ( 0.000000000000000000, -0.7091011189803928527, 0.7051068025914618564 ) ) ;
#5966 = CIRCLE ( 'NONE', #758, 7.000000000000006217 ) ;
#5967 = VECTOR ( 'NONE', #6181, 1000.000000000000114 ) ;
#5968 = ORIENTED_EDGE ( 'NONE', *, *, #7710, .T. ) ;
#5969 = FACE_OUTER_BOUND ( 'NONE', #12224, .T. ) ;
#5970 = VECTOR ( 'NONE', #5588, 1000.000000000000000 ) ;
#5971 = ORIENTED_EDGE ( 'NONE', *, *, #725, .T. ) ;
#5972 = DIRECTION ( 'NONE',  ( 1.000000000000000000, 0.000000000000000000, -0.000000000000000000 ) ) ;
#5973 = ORIENTED_EDGE ( 'NONE', *, *, #10732, .T. ) ;
#5974 = AXIS2_PLACEMENT_3D ( 'NONE', #2726, #8606, #12283 ) ;
#5975 = CIRCLE ( 'NONE', #8777, 9.600000000009600853 ) ;
#5976 = DIRECTION ( 'NONE',  ( -1.000000000000000000, 0.000000000000000000, 0.000000000000000000 ) ) ;
#5977 = ORIENTED_EDGE ( 'NONE', *, *, #9917, .T. ) ;
#5978 = DIRECTION ( 'NONE',  ( 1.000000000000000000, 0.000000000000000000, 0.000000000000000000 ) ) ;
#5979 = CARTESIAN_POINT ( 'NONE',  ( 37.00000000000000711, -2.432816653220593039, 4.137801726981678030 ) ) ;
#5980 = DIRECTION ( 'NONE',  ( -1.000000000000000000, -0.000000000000000000, -0.000000000000000000 ) ) ;
#5981 = DIRECTION ( 'NONE',  ( 0.000000000000000000, 0.000000000000000000, -1.000000000000000000 ) ) ;
#5982 = EDGE_LOOP ( 'NONE', ( #5740, #5559, #10057, #1052 ) ) ;
#5983 = AXIS2_PLACEMENT_3D ( 'NONE', #11507, #4652, #10575 ) ;
#5984 = VERTEX_POINT ( 'NONE', #8178 ) ;
#5985 = CIRCLE ( 'NONE', #4764, 2.041999999999999815 ) ;
#5986 = ORIENTED_EDGE ( 'NONE', *, *, #6261, .T. ) ;
#5987 = CLOSED_SHELL ( 'NONE', ( #59, #4885, #5687, #7949, #10675, #8306 ) ) ;
#5988 = CYLINDRICAL_SURFACE ( 'NONE', #8423, 25.00000000000000000 ) ;
#5989 = EDGE_LOOP ( 'NONE', ( #4518, #7697, #3172, #5788 ) ) ;
#5990 = DIRECTION ( 'NONE',  ( 0.000000000000000000, -0.5000000000000072164, 0.8660254037844345998 ) ) ;
#5991 = CIRCLE ( 'NONE', #11560, 0.7500000000000000000 ) ;
#5992 = DIRECTION ( 'NONE',  ( 1.000000000000000000, 0.000000000000000000, 0.000000000000000000 ) ) ;
#5993 = EDGE_CURVE ( 'NONE', #4722, #7798, #7119, .T. ) ;
#5994 = AXIS2_PLACEMENT_3D ( 'NONE', #10008, #11865, #10880 ) ;
#5995 = EDGE_CURVE ( 'NONE', #8081, #7435, #2419, .T. ) ;
#5996 = ORIENTED_EDGE ( 'NONE', *, *, #2037, .F. ) ;
#5997 = CARTESIAN_POINT ( 'NONE',  ( 36.00000000000000000, 40.00000000000000711, -19.99999999999998934 ) ) ;
#5998 = DIRECTION ( 'NONE',  ( 1.000000000000000000, 0.000000000000000000, 0.000000000000000000 ) ) ;
#5999 = EDGE_LOOP ( 'NONE', ( #10242, #10287, #11061, #2282 ) ) ;
#6000 =( LENGTH_UNIT ( ) NAMED_UNIT ( * ) SI_UNIT ( .MILLI., .METRE. ) );
#6001 = FILL_AREA_STYLE_COLOUR ( '', #11794 ) ;
#6002 = DIRECTION ( 'NONE',  ( 1.000000000000000000, 0.000000000000000000, 0.000000000000000000 ) ) ;
#6003 = AXIS2_PLACEMENT_3D ( 'NONE', #8965, #5202, #7032 ) ;
#6004 = DIRECTION ( 'NONE',  ( 0.000000000000000000, 0.000000000000000000, 1.000000000000000000 ) ) ;
#6005 = AXIS2_PLACEMENT_3D ( 'NONE', #3506, #11065, #2499 ) ;
#6006 = ORIENTED_EDGE ( 'NONE', *, *, #1519, .F. ) ;
#6007 = CARTESIAN_POINT ( 'NONE',  ( 4.999999999999999112, 19.60720892790252989, -11.14352537685181588 ) ) ;
#6008 = AXIS2_PLACEMENT_3D ( 'NONE', #8888, #3311, #3360 ) ;
#6009 = FILL_AREA_STYLE_COLOUR ( '', #10380 ) ;
#6010 = EDGE_CURVE ( 'NONE', #214, #4309, #7360, .T. ) ;
#6011=STYLED_ITEM('',(#12405),#8778);
#6012 = CARTESIAN_POINT ( 'NONE',  ( 45.00000000000001421, 5.744562646538041051, -38.00000000000000000 ) ) ;
#6013 = DIRECTION ( 'NONE',  ( -1.000000000000000000, -0.000000000000000000, -0.000000000000000000 ) ) ;
#6014 = ADVANCED_FACE ( 'NONE', ( #6356, #671 ), #4414, .F. ) ;
#6015 = VECTOR ( 'NONE', #3408, 1000.000000000000000 ) ;
#6016 = EDGE_CURVE ( 'NONE', #10133, #11838, #11102, .T. ) ;
#6017 = CIRCLE ( 'NONE', #1817, 0.7500000000000000000 ) ;
#6018 = DIRECTION ( 'NONE',  ( -1.000000000000000000, -0.000000000000000000, -0.000000000000000000 ) ) ;
#6019 = DIRECTION ( 'NONE',  ( 0.000000000000000000, 0.000000000000000000, -1.000000000000000000 ) ) ;
#6020 = EDGE_CURVE ( 'NONE', #10868, #1819, #9825, .T. ) ;
#6021 = EDGE_LOOP ( 'NONE', ( #594, #7973, #3350, #9599 ) ) ;
#6022 = CARTESIAN_POINT ( 'NONE',  ( 2.499999999999998668, 20.13931372320397273, -5.950465759858654557 ) ) ;
#6023 = DIRECTION ( 'NONE',  ( -1.000000000000000000, -0.000000000000000000, -0.000000000000000000 ) ) ;
#6024 = ORIENTED_EDGE ( 'NONE', *, *, #2116, .T. ) ;
#6025 = LINE ( 'NONE', #379, #2893 ) ;
#6026 =( REPRESENTATION_RELATIONSHIP ('NONE','NONE', #9709, #1953 ) REPRESENTATION_RELATIONSHIP_WITH_TRANSFORMATION ( #10532 )SHAPE_REPRESENTATION_RELATIONSHIP( ) );
#6027 = PRODUCT_DEFINITION_CONTEXT ( 'detailed design', #3934, 'design' ) ;
#6028 = VERTEX_POINT ( 'NONE', #8302 ) ;
#6029 = CYLINDRICAL_SURFACE ( 'NONE', #8636, 21.00000000002100009 ) ;
#6030 = CIRCLE ( 'NONE', #616, 7.000000000000000000 ) ;
#6031 = AXIS2_PLACEMENT_3D ( 'NONE', #12259, #3586, #3526 ) ;
#6032 = AXIS2_PLACEMENT_3D ( 'NONE', #3120, #4795, #5798 ) ;
#6033 = EDGE_CURVE ( 'NONE', #8470, #2779, #11403, .T. ) ;
#6034 = CARTESIAN_POINT ( 'NONE',  ( 2.354826896168714434, -6.962563485461402024, -1.000000000000000000 ) ) ;
#6035 = LINE ( 'NONE', #11649, #6962 ) ;
#6036 = CARTESIAN_POINT ( 'NONE',  ( 4.999999999999999112, 17.79862902732265084, 13.85025647830063100 ) ) ;
#6037 = FACE_OUTER_BOUND ( 'NONE', #11509, .T. ) ;
#6038 = CIRCLE ( 'NONE', #6638, 9.600000000009599077 ) ;
#6039 = ORIENTED_EDGE ( 'NONE', *, *, #666, .F. ) ;
#6040 = EDGE_LOOP ( 'NONE', ( #9176, #11357, #4869, #2789 ) ) ;
#6041 = DIRECTION ( 'NONE',  ( 0.000000000000000000, 0.000000000000000000, 1.000000000000000000 ) ) ;
#6042 = ORIENTED_EDGE ( 'NONE', *, *, #4117, .F. ) ;
#6043 = AXIS2_PLACEMENT_3D ( 'NONE', #7149, #9104, #1327 ) ;
#6044 = AXIS2_PLACEMENT_3D ( 'NONE', #6183, #8946, #2247 ) ;
#6045 = ADVANCED_FACE ( 'NONE', ( #10165 ), #11966, .T. ) ;
#6046 = CIRCLE ( 'NONE', #2242, 7.200000000007202416 ) ;
#6047 = DIRECTION ( 'NONE',  ( -1.000000000000000000, -0.000000000000000000, 0.000000000000000000 ) ) ;
#6048 = DIRECTION ( 'NONE',  ( 0.000000000000000000, -0.7071067811865536790, 0.7071067811865413555 ) ) ;
#6049 = CARTESIAN_POINT ( 'NONE',  ( 50.00005079999999680, 0.000000000000000000, 1.500000000000000000 ) ) ;
#6050 = DIRECTION ( 'NONE',  ( 0.000000000000000000, 0.000000000000000000, 1.000000000000000000 ) ) ;
#6051 = DIRECTION ( 'NONE',  ( -1.000000000000000000, 0.000000000000000000, 0.000000000000000000 ) ) ;
#6052 = ORIENTED_EDGE ( 'NONE', *, *, #10118, .T. ) ;
#6053 = AXIS2_PLACEMENT_3D ( 'NONE', #1411, #8990, #10111 ) ;
#6054 = CIRCLE ( 'NONE', #653, 9.600000000009600853 ) ;
#6055 = VERTEX_POINT ( 'NONE', #8069 ) ;
#6056 = AXIS2_PLACEMENT_3D ( 'NONE', #212, #4035, #8864 ) ;
#6057 = SURFACE_SIDE_STYLE ('',( #113 ) ) ;
#6058 = AXIS2_PLACEMENT_3D ( 'NONE', #11993, #2551, #8270 ) ;
#6059 = VERTEX_POINT ( 'NONE', #2295 ) ;
#6060 = DIRECTION ( 'NONE',  ( 1.000000000000000000, 0.000000000000000000, 0.000000000000000000 ) ) ;
#6061 = DIRECTION ( 'NONE',  ( -1.000000000000000000, 0.000000000000000000, 0.000000000000000000 ) ) ;
#6062 = LINE ( 'NONE', #7996, #7806 ) ;
#6063 = CIRCLE ( 'NONE', #669, 5.999999999999999112 ) ;
#6064 = ORIENTED_EDGE ( 'NONE', *, *, #8478, .F. ) ;
#6065 = DIRECTION ( 'NONE',  ( 0.000000000000000000, 0.000000000000000000, 1.000000000000000000 ) ) ;
#6066 = CARTESIAN_POINT ( 'NONE',  ( 0.000000000000000000, 1.178949249685213863, -2.042000000000001148 ) ) ;
#6067 = VERTEX_POINT ( 'NONE', #9250 ) ;
#6068 = PLANE ( 'NONE',  #9466 ) ;
#6069 = DIRECTION ( 'NONE',  ( 0.000000000000000000, 0.000000000000000000, -1.000000000000000000 ) ) ;
#6070 = DIRECTION ( 'NONE',  ( -1.000000000000000000, -0.000000000000000000, -0.000000000000000000 ) ) ;
#6071 = EDGE_CURVE ( 'NONE', #4594, #997, #5356, .T. ) ;
#6072 =( GEOMETRIC_REPRESENTATION_CONTEXT ( 3 ) GLOBAL_UNCERTAINTY_ASSIGNED_CONTEXT ( ( #8407 ) ) GLOBAL_UNIT_ASSIGNED_CONTEXT ( ( #6000, #5119, #6892 ) ) REPRESENTATION_CONTEXT ( 'NONE', 'WORKASPACE' ) );
#6073 = ORIENTED_EDGE ( 'NONE', *, *, #7851, .T. ) ;
#6074 = CARTESIAN_POINT ( 'NONE',  ( -0.2500000000000000000, -8.096141056083446585, 0.000000000000000000 ) ) ;
#6075 = EDGE_CURVE ( 'NONE', #4941, #6339, #12092, .T. ) ;
#6076 = CARTESIAN_POINT ( 'NONE',  ( 4.999999999999999112, -22.37914155802287297, 2.791921004064167544 ) ) ;
#6077 = FACE_OUTER_BOUND ( 'NONE', #10669, .T. ) ;
#6078 = DIRECTION ( 'NONE',  ( 0.000000000000000000, 0.000000000000000000, 1.000000000000000000 ) ) ;
#6079 = AXIS2_PLACEMENT_3D ( 'NONE', #5094, #10850, #11706 ) ;
#6080 = DIRECTION ( 'NONE',  ( 0.000000000000000000, 0.9238795325112877377, -0.3826834323650873393 ) ) ;
#6081 = CARTESIAN_POINT ( 'NONE',  ( 0.000000000000000000, 0.000000000000000000, 0.000000000000000000 ) ) ;
#6082 = ORIENTED_EDGE ( 'NONE', *, *, #4936, .F. ) ;
#6083 = VERTEX_POINT ( 'NONE', #10058 ) ;
#6084 = DIRECTION ( 'NONE',  ( -1.000000000000000000, -0.000000000000000000, -0.000000000000000000 ) ) ;
#6085 = CARTESIAN_POINT ( 'NONE',  ( 4.999999999999999112, 13.17168466712928598, 15.37949036966216632 ) ) ;
#6086 = ORIENTED_EDGE ( 'NONE', *, *, #8612, .T. ) ;
#6087 = DIRECTION ( 'NONE',  ( -1.000000000000000000, -3.903127820947815962E-18, 0.000000000000000000 ) ) ;
#6088 = EDGE_CURVE ( 'NONE', #9230, #6352, #6419, .T. ) ;
#6089 = EDGE_LOOP ( 'NONE', ( #12305, #5679, #8687, #8501 ) ) ;
#6090 = CARTESIAN_POINT ( 'NONE',  ( 0.000000000000000000, 15.37949036966211835, 13.17168466712934105 ) ) ;
#6091 = EDGE_CURVE ( 'NONE', #9587, #3084, #3357, .T. ) ;
#6092 = AXIS2_PLACEMENT_3D ( 'NONE', #7906, #9777, #8776 ) ;
#6093 = ADVANCED_FACE ( 'NONE', ( #5599 ), #8021, .T. ) ;
#6094 = CARTESIAN_POINT ( 'NONE',  ( 15.00000000000000355, 44.00000000000001421, 0.000000000000000000 ) ) ;
#6095 = DIRECTION ( 'NONE',  ( 0.000000000000000000, -1.000000000000000000, -1.048062100068272767E-14 ) ) ;
#6096 = CARTESIAN_POINT ( 'NONE',  ( -33.00000000000000000, 0.000000000000000000, 0.000000000000000000 ) ) ;
#6097 = ORIENTED_EDGE ( 'NONE', *, *, #6781, .F. ) ;
#6098 = AXIS2_PLACEMENT_3D ( 'NONE', #7207, #6203, #8205 ) ;
#6099 = DIRECTION ( 'NONE',  ( 0.000000000000000000, 0.000000000000000000, 1.000000000000000000 ) ) ;
#6100 = AXIS2_PLACEMENT_3D ( 'NONE', #4383, #8212, #12008 ) ;
#6101 = EDGE_LOOP ( 'NONE', ( #7331, #2744, #8546, #5255 ) ) ;
#6102 = CARTESIAN_POINT ( 'NONE',  ( -15.00000000000000000, 44.00000000000001421, -2.149999999999999023 ) ) ;
#6103 = EDGE_LOOP ( 'NONE', ( #2019, #11159, #11832, #7820, #5081, #10530, #281, #1711 ) ) ;
#6104 = PRODUCT_RELATED_PRODUCT_CATEGORY ( 'part', '', ( #9134 ) ) ;
#6105 = VECTOR ( 'NONE', #11236, 1000.000000000000000 ) ;
#6106 = DIRECTION ( 'NONE',  ( 0.000000000000000000, 0.000000000000000000, 1.000000000000000000 ) ) ;
#6107 = CARTESIAN_POINT ( 'NONE',  ( 2.499999999999999556, 14.41081992069341133, -22.83261415639488234 ) ) ;
#6108 = CARTESIAN_POINT ( 'NONE',  ( 0.3688486069976970039, 0.6000000000000000888, -3.516473936516294252 ) ) ;
#6109 = CARTESIAN_POINT ( 'NONE',  ( 0.000000000000000000, 0.000000000000000000, 0.000000000000000000 ) ) ;
#6110 = PLANE ( 'NONE',  #11390 ) ;
#6111 = EDGE_LOOP ( 'NONE', ( #11130, #2420, #2494, #5404, #540, #1559 ) ) ;
#6112 = DIRECTION ( 'NONE',  ( 1.000000000000000000, 0.000000000000000000, 0.000000000000000000 ) ) ;
#6113 = VERTEX_POINT ( 'NONE', #1727 ) ;
#6114 = EDGE_CURVE ( 'NONE', #4049, #2452, #4673, .T. ) ;
#6116 = ADVANCED_FACE ( 'NONE', ( #12148, #8548 ), #2597, .T. ) ;
#6115 = ORIENTED_EDGE ( 'NONE', *, *, #5554, .F. ) ;
#6117 = CARTESIAN_POINT ( 'NONE',  ( 33.00000000000000000, 9.184850993605147944E-16, -34.49999999999999289 ) ) ;
#6118 = CARTESIAN_POINT ( 'NONE',  ( 26.00000000000000355, 7.347880794884119736E-16, -35.99999999999999289 ) ) ;
#6119 = CARTESIAN_POINT ( 'NONE',  ( 43.00000000000000000, 0.000000000000000000, 5.000000000000000000 ) ) ;
#6120 = EDGE_LOOP ( 'NONE', ( #4748, #1648, #1231, #1121 ) ) ;
#6121 = DIRECTION ( 'NONE',  ( 0.000000000000000000, -0.7071067811865536790, 0.7071067811865413555 ) ) ;
#6122 = ORIENTED_EDGE ( 'NONE', *, *, #5463, .F. ) ;
#6123 = CARTESIAN_POINT ( 'NONE',  ( 0.000000000000000000, 0.5192545390863916310, -1.000000000000000000 ) ) ;
#6124 = CARTESIAN_POINT ( 'NONE',  ( 4.999999999999999112, 0.000000000000000000, 0.000000000000000000 ) ) ;
#6125 = VERTEX_POINT ( 'NONE', #6423 ) ;
#6126 = CYLINDRICAL_SURFACE ( 'NONE', #8584, 6.000000000000005329 ) ;
#6127 = PRODUCT ( 'main body', 'main body', '', ( #100 ) ) ;
#6128 = DIRECTION ( 'NONE',  ( 1.000000000000000000, 0.000000000000000000, 0.000000000000000000 ) ) ;
#6129 = CARTESIAN_POINT ( 'NONE',  ( 36.00000000000000711, -12.50000000000000000, -37.99671038392666134 ) ) ;
#6130 = CARTESIAN_POINT ( 'NONE',  ( 51.00000000000000000, 0.000000000000000000, -41.99999999999999289 ) ) ;
#6131 = DIRECTION ( 'NONE',  ( 0.000000000000000000, 1.000000000000000000, 0.000000000000000000 ) ) ;
#6132 = CYLINDRICAL_SURFACE ( 'NONE', #3256, 7.200000000007204193 ) ;
#6133 = ORIENTED_EDGE ( 'NONE', *, *, #5700, .F. ) ;
#6134 = ORIENTED_EDGE ( 'NONE', *, *, #4179, .T. ) ;
#6135 = ADVANCED_FACE ( 'NONE', ( #1787 ), #11196, .T. ) ;
#6136 = DIRECTION ( 'NONE',  ( -1.000000000000000000, 0.000000000000000000, 0.000000000000000000 ) ) ;
#6137 = CARTESIAN_POINT ( 'NONE',  ( 0.000000000000000000, 0.000000000000000000, -1.500000000000000000 ) ) ;
#6138 = ORIENTED_EDGE ( 'NONE', *, *, #498, .F. ) ;
#6139 = DIRECTION ( 'NONE',  ( 0.000000000000000000, 0.000000000000000000, 1.000000000000000000 ) ) ;
#6140 = PRODUCT_DEFINITION_CONTEXT ( 'detailed design', #3073, 'design' ) ;
#6141 = ORIENTED_EDGE ( 'NONE', *, *, #6075, .F. ) ;
#6142 = DIRECTION ( 'NONE',  ( -1.000000000000000000, 0.000000000000000000, 0.000000000000000000 ) ) ;
#6143 = PRESENTATION_STYLE_ASSIGNMENT (( #9100 ) ) ;
#6144 = CARTESIAN_POINT ( 'NONE',  ( -31.74999999999995737, 0.000000000000000000, 4.250000000000000000 ) ) ;
#6145 = EDGE_CURVE ( 'NONE', #10175, #4256, #9423, .T. ) ;
#6146 = DIRECTION ( 'NONE',  ( -0.000000000000000000, 1.000000000000000000, -0.000000000000000000 ) ) ;
#6147 = CARTESIAN_POINT ( 'NONE',  ( 0.1481481481481481122, -4.797713218419819903, -1.000000000000000000 ) ) ;
#6148 = ORIENTED_EDGE ( 'NONE', *, *, #7490, .T. ) ;
#6149 = ADVANCED_FACE ( 'NONE', ( #2725 ), #913, .T. ) ;
#6150 = FACE_OUTER_BOUND ( 'NONE', #8555, .T. ) ;
#6151 = ADVANCED_FACE ( 'NONE', ( #11409 ), #7545, .T. ) ;
#6152 = ORIENTED_EDGE ( 'NONE', *, *, #6176, .F. ) ;
#6153 = CARTESIAN_POINT ( 'NONE',  ( 43.00000000000000000, 6.123233995736765296E-16, -5.000000000000000000 ) ) ;
#6154 = VERTEX_POINT ( 'NONE', #3787 ) ;
#6155 = FACE_OUTER_BOUND ( 'NONE', #2522, .T. ) ;
#6156 = AXIS2_PLACEMENT_3D ( 'NONE', #12235, #10550, #6699 ) ;
#6157 = CARTESIAN_POINT ( 'NONE',  ( 0.000000000000000000, -22.83261415639492498, -14.41081992069334561 ) ) ;
#6158 = LINE ( 'NONE', #11897, #11391 ) ;
#6159 = VECTOR ( 'NONE', #8395, 1000.000000000000000 ) ;
#6160 = CYLINDRICAL_SURFACE ( 'NONE', #8036, 5.000000000000000000 ) ;
#6161 = CARTESIAN_POINT ( 'NONE',  ( 43.00000000000000000, -3.185523555419110586, 3.853886308373666747 ) ) ;
#6162 = ORIENTED_EDGE ( 'NONE', *, *, #10700, .F. ) ;
#6163 = ADVANCED_FACE ( 'NONE', ( #1860 ), #11160, .T. ) ;
#6164 = EDGE_CURVE ( 'NONE', #7890, #170, #6831, .T. ) ;
#6165 = CARTESIAN_POINT ( 'NONE',  ( 36.00000000000000711, -4.104405154062230115E-16, -2.224720805914714718E-17 ) ) ;
#6166 = EDGE_CURVE ( 'NONE', #710, #7137, #1435, .T. ) ;
#6167 = ORIENTED_EDGE ( 'NONE', *, *, #10800, .T. ) ;
#6168 = DIRECTION ( 'NONE',  ( 1.000000000000000000, 0.000000000000000000, 0.000000000000000000 ) ) ;
#6169 = ORIENTED_EDGE ( 'NONE', *, *, #1712, .T. ) ;
#6171 = CARTESIAN_POINT ( 'NONE',  ( 4.999999999999999112, -19.60720892790260805, 11.14352537685167732 ) ) ;
#6170 = CIRCLE ( 'NONE', #5372, 7.500000000000000888 ) ;
#6172 = CIRCLE ( 'NONE', #767, 7.000000000000000000 ) ;
#6173 = DIRECTION ( 'NONE',  ( 0.000000000000000000, 0.000000000000000000, 1.000000000000000000 ) ) ;
#6174 = ORIENTED_EDGE ( 'NONE', *, *, #11426, .F. ) ;
#6175 = PLANE ( 'NONE',  #7607 ) ;
#6176 = EDGE_CURVE ( 'NONE', #11838, #3551, #8355, .T. ) ;
#6177 = ADVANCED_FACE ( 'NONE', ( #9308 ), #4538, .T. ) ;
#6178 = AXIS2_PLACEMENT_3D ( 'NONE', #10174, #7369, #10297 ) ;
#6179 = EDGE_LOOP ( 'NONE', ( #11167, #9671, #1856, #8320 ) ) ;
#6180 = CIRCLE ( 'NONE', #582, 9.600000000009599077 ) ;
#6181 = DIRECTION ( 'NONE',  ( -2.731402571913187487E-17, -0.5883347247165658933, 0.8086174940555531654 ) ) ;
#6182 = ORIENTED_EDGE ( 'NONE', *, *, #6452, .T. ) ;
#6183 = CARTESIAN_POINT ( 'NONE',  ( 1.399999999999998579, 0.000000000000000000, 0.000000000000000000 ) ) ;
#6184 = DIRECTION ( 'NONE',  ( 0.000000000000000000, 0.000000000000000000, 1.000000000000000000 ) ) ;
#6185 = ORIENTED_EDGE ( 'NONE', *, *, #9742, .T. ) ;
#6186 = CARTESIAN_POINT ( 'NONE',  ( 4.999999999999999112, 0.000000000000000000, 0.000000000000000000 ) ) ;
#6187 = CIRCLE ( 'NONE', #2194, 9.600000000009600853 ) ;
#6188 = AXIS2_PLACEMENT_3D ( 'NONE', #11863, #8829, #1129 ) ;
#6189 = CIRCLE ( 'NONE', #3391, 9.600000000009600853 ) ;
#6190 = SURFACE_SIDE_STYLE ('',( #10819 ) ) ;
#6191 = EDGE_CURVE ( 'NONE', #9147, #170, #4602, .T. ) ;
#6192 = CARTESIAN_POINT ( 'NONE',  ( 2.500000000000000000, 2.357898499370433054, -1.951563910473907981E-15 ) ) ;
#6193 = DIRECTION ( 'NONE',  ( 1.000000000000000000, 0.000000000000000000, 0.000000000000000000 ) ) ;
#6194 = CARTESIAN_POINT ( 'NONE',  ( 4.999999999999997335, 0.000000000000000000, 0.000000000000000000 ) ) ;
#6195 = DIRECTION ( 'NONE',  ( 0.000000000000000000, 0.6828850436591804574, 0.7305258497456468270 ) ) ;
#6196 = VECTOR ( 'NONE', #700, 1000.000000000000000 ) ;
#6197 = ORIENTED_EDGE ( 'NONE', *, *, #174, .T. ) ;
#6198 = VERTEX_POINT ( 'NONE', #8780 ) ;
#6199 = DIRECTION ( 'NONE',  ( 0.000000000000000000, 0.000000000000000000, -1.000000000000000000 ) ) ;
#6200 = LINE ( 'NONE', #9093, #7834 ) ;
#6201 = VECTOR ( 'NONE', #4169, 1000.000000000000000 ) ;
#6202 = ORIENTED_EDGE ( 'NONE', *, *, #11477, .F. ) ;
#6203 = DIRECTION ( 'NONE',  ( -1.000000000000000000, 0.000000000000000000, 0.000000000000000000 ) ) ;
#6204 = ORIENTED_EDGE ( 'NONE', *, *, #7715, .T. ) ;
#6205 = CARTESIAN_POINT ( 'NONE',  ( 25.00000000000000000, 0.000000000000000000, -25.00000000000000000 ) ) ;
#6206 = VECTOR ( 'NONE', #9576, 1000.000000000000000 ) ;
#6207 = VECTOR ( 'NONE', #10823, 999.9999999999998863 ) ;
#6208 = ORIENTED_EDGE ( 'NONE', *, *, #10760, .F. ) ;
#6209 = AXIS2_PLACEMENT_3D ( 'NONE', #2223, #9871, #4218 ) ;
#6210 = CARTESIAN_POINT ( 'NONE',  ( 2.500000000000000000, -1.178949249685213863, 2.042000000000002924 ) ) ;
#6211 = DIRECTION ( 'NONE',  ( 0.000000000000000000, 0.000000000000000000, 1.000000000000000000 ) ) ;
#6212 = DIRECTION ( 'NONE',  ( 0.000000000000000000, 0.000000000000000000, -1.000000000000000000 ) ) ;
#6213 = ORIENTED_EDGE ( 'NONE', *, *, #2065, .F. ) ;
#6214 = DIRECTION ( 'NONE',  ( 0.000000000000000000, 0.000000000000000000, 1.000000000000000000 ) ) ;
#6215 = DIRECTION ( 'NONE',  ( -1.000000000000000000, 0.000000000000000000, 0.000000000000000000 ) ) ;
#6216 = MECHANICAL_DESIGN_GEOMETRIC_PRESENTATION_REPRESENTATION (  '', ( #6011 ), #7813 ) ;
#6217 = ORIENTED_EDGE ( 'NONE', *, *, #7379, .T. ) ;
#6218 = DIRECTION ( 'NONE',  ( 0.000000000000000000, 0.000000000000000000, -1.000000000000000000 ) ) ;
#6219 = CIRCLE ( 'NONE', #6826, 7.200000000007202416 ) ;
#6220 = ORIENTED_EDGE ( 'NONE', *, *, #2628, .F. ) ;
#6221 = CIRCLE ( 'NONE', #6830, 9.600000000009600853 ) ;
#6222 = AXIS2_PLACEMENT_3D ( 'NONE', #5057, #4162, #7991 ) ;
#6223 = EDGE_CURVE ( 'NONE', #9343, #10133, #8038, .T. ) ;
#6224 = EDGE_CURVE ( 'NONE', #1927, #7407, #3628, .T. ) ;
#6225 = SURFACE_SIDE_STYLE ('',( #9233 ) ) ;
#6226 = VECTOR ( 'NONE', #2791, 1000.000000000000000 ) ;
#6227 = AXIS2_PLACEMENT_3D ( 'NONE', #12115, #8275, #6569 ) ;
#6228 = FACE_OUTER_BOUND ( 'NONE', #5265, .T. ) ;
#6229 = DIRECTION ( 'NONE',  ( -1.000000000000000000, 0.000000000000000000, -0.000000000000000000 ) ) ;
#6230 = AXIS2_PLACEMENT_3D ( 'NONE', #6096, #3288, #6212 ) ;
#6231 = VECTOR ( 'NONE', #11078, 1000.000000000000000 ) ;
#6232 = CARTESIAN_POINT ( 'NONE',  ( 5.000000000000000888, 0.000000000000000000, 0.000000000000000000 ) ) ;
#6233 = DIRECTION ( 'NONE',  ( 0.000000000000000000, 0.000000000000000000, -1.000000000000000000 ) ) ;
#6234 = ORIENTED_EDGE ( 'NONE', *, *, #502, .T. ) ;
#6235 = CARTESIAN_POINT ( 'NONE',  ( 4.999999999999999112, 11.41582255376072830, 8.527191590521114861 ) ) ;
#6236 = ORIENTED_EDGE ( 'NONE', *, *, #1783, .F. ) ;
#6237 = DIRECTION ( 'NONE',  ( -1.000000000000000000, -6.162975822039154730E-33, -1.927882050300263517E-17 ) ) ;
#6238 = VERTEX_POINT ( 'NONE', #10711 ) ;
#6239 = VECTOR ( 'NONE', #10400, 1000.000000000000000 ) ;
#6240 = DIRECTION ( 'NONE',  ( 0.000000000000000000, 1.000000000000000000, 0.000000000000000000 ) ) ;
#6241 = AXIS2_PLACEMENT_3D ( 'NONE', #6165, #8987, #4158 ) ;
#6242 = EDGE_CURVE ( 'NONE', #1333, #10309, #5017, .T. ) ;
#6243 = AXIS2_PLACEMENT_3D ( 'NONE', #2701, #10321, #2514 ) ;
#6244 = DIRECTION ( 'NONE',  ( 0.000000000000000000, 0.000000000000000000, 1.000000000000000000 ) ) ;
#6245 = ADVANCED_FACE ( 'NONE', ( #1382, #511 ), #273, .T. ) ;
#6246 = ADVANCED_FACE ( 'NONE', ( #9097 ), #10942, .F. ) ;
#6247 = EDGE_CURVE ( 'NONE', #9598, #1449, #7639, .T. ) ;
#6248 = ORIENTED_EDGE ( 'NONE', *, *, #4055, .T. ) ;
#6249 = CARTESIAN_POINT ( 'NONE',  ( -1.399999999999999689, 0.000000000000000000, 0.000000000000000000 ) ) ;
#6250 = AXIS2_PLACEMENT_3D ( 'NONE', #12145, #6604, #5669 ) ;
#6251 =( GEOMETRIC_REPRESENTATION_CONTEXT ( 3 ) GLOBAL_UNCERTAINTY_ASSIGNED_CONTEXT ( ( #11511 ) ) GLOBAL_UNIT_ASSIGNED_CONTEXT ( ( #2556, #6270, #2625 ) ) REPRESENTATION_CONTEXT ( 'NONE', 'WORKASPACE' ) );
#6252 = ORIENTED_EDGE ( 'NONE', *, *, #2884, .F. ) ;
#6253 = CIRCLE ( 'NONE', #10438, 9.600000000009602630 ) ;
#6254 = DIRECTION ( 'NONE',  ( 0.000000000000000000, 0.000000000000000000, 1.000000000000000000 ) ) ;
#6255 = ORIENTED_EDGE ( 'NONE', *, *, #3254, .F. ) ;
#6256 =( NAMED_UNIT ( * ) PLANE_ANGLE_UNIT ( ) SI_UNIT ( $, .RADIAN. ) );
#6257 = DIRECTION ( 'NONE',  ( 1.000000000000000000, -0.000000000000000000, -0.000000000000000000 ) ) ;
#6258 = ORIENTED_EDGE ( 'NONE', *, *, #7159, .F. ) ;
#6259 = CARTESIAN_POINT ( 'NONE',  ( 4.999999999999999112, 14.40062958310465469, -1.672489362011036595 ) ) ;
#6260 = AXIS2_PLACEMENT_3D ( 'NONE', #11923, #7332, #10187 ) ;
#6261 = EDGE_CURVE ( 'NONE', #8991, #3326, #1461, .T. ) ;
#6262 = DIRECTION ( 'NONE',  ( 0.000000000000000000, 0.000000000000000000, -1.000000000000000000 ) ) ;
#6263 = LINE ( 'NONE', #7134, #404 ) ;
#6264 = CARTESIAN_POINT ( 'NONE',  ( 1.400000000000000133, 0.000000000000000000, 0.000000000000000000 ) ) ;
#6265 = DIRECTION ( 'NONE',  ( -0.000000000000000000, -0.000000000000000000, -1.000000000000000000 ) ) ;
#6266 = VERTEX_POINT ( 'NONE', #9906 ) ;
#6267 = ORIENTED_EDGE ( 'NONE', *, *, #3795, .F. ) ;
#6268 = CARTESIAN_POINT ( 'NONE',  ( 42.00000000000000000, -2.003605614753219590E-16, 0.000000000000000000 ) ) ;
#6269 = CIRCLE ( 'NONE', #7278, 7.200000000007200640 ) ;
#6270 =( NAMED_UNIT ( * ) PLANE_ANGLE_UNIT ( ) SI_UNIT ( $, .RADIAN. ) );
#6271 = DIRECTION ( 'NONE',  ( 1.000000000000000000, 0.000000000000000000, 0.000000000000000000 ) ) ;
#6272 = ORIENTED_EDGE ( 'NONE', *, *, #6166, .F. ) ;
#6273 = DIRECTION ( 'NONE',  ( 1.000000000000000000, 0.000000000000000000, 0.000000000000000000 ) ) ;
#6274 = ADVANCED_FACE ( 'NONE', ( #1323 ), #6029, .T. ) ;
#6275 = ORIENTED_EDGE ( 'NONE', *, *, #9919, .F. ) ;
#6276 = PLANE ( 'NONE',  #11613 ) ;
#6277 = EDGE_CURVE ( 'NONE', #4273, #7263, #1640, .T. ) ;
#6278=STYLED_ITEM('',(#12391),#4548);
#6279 = ORIENTED_EDGE ( 'NONE', *, *, #9761, .T. ) ;
#6280 = CARTESIAN_POINT ( 'NONE',  ( 4.999999999999999112, 9.168210874537823685, -18.05452603534156353 ) ) ;
#6281 = LINE ( 'NONE', #2456, #6159 ) ;
#6282 = CARTESIAN_POINT ( 'NONE',  ( 4.999999999999999112, 20.13931372320397273, -5.950465759858656334 ) ) ;
#6283 = CARTESIAN_POINT ( 'NONE',  ( -1.500000000000001332, 0.000000000000000000, 0.000000000000000000 ) ) ;
#6284 = ORIENTED_EDGE ( 'NONE', *, *, #8797, .F. ) ;
#6285 = DIRECTION ( 'NONE',  ( -0.000000000000000000, 1.000000000000000000, -0.000000000000000000 ) ) ;
#6286 = CARTESIAN_POINT ( 'NONE',  ( 0.000000000000000000, 6.799999999999999822, 1.500000000000000000 ) ) ;
#6287 = ORIENTED_EDGE ( 'NONE', *, *, #12029, .F. ) ;
#6288 = DIRECTION ( 'NONE',  ( -0.000000000000000000, 1.000000000000000000, -0.000000000000000000 ) ) ;
#6289 = AXIS2_PLACEMENT_3D ( 'NONE', #9028, #10192, #10021 ) ;
#6290 = ORIENTED_EDGE ( 'NONE', *, *, #10597, .T. ) ;
#6291 = DIRECTION ( 'NONE',  ( 1.000000000000000000, 0.000000000000000000, 0.000000000000000000 ) ) ;
#6292 = DIRECTION ( 'NONE',  ( 1.000000000000000000, 0.000000000000000000, 0.000000000000000000 ) ) ;
#6293 = CARTESIAN_POINT ( 'NONE',  ( -13.05124837953327344, 0.000000000000000000, -54.50000000000000000 ) ) ;
#6294 = VECTOR ( 'NONE', #5384, 1000.000000000000000 ) ;
#6295 = CARTESIAN_POINT ( 'NONE',  ( 36.00000000000000000, 0.000000000000000000, -41.99999999999999289 ) ) ;
#6296 = DIRECTION ( 'NONE',  ( 0.000000000000000000, 0.000000000000000000, -1.000000000000000000 ) ) ;
#6297 = VERTEX_POINT ( 'NONE', #11699 ) ;
#6298 = DIRECTION ( 'NONE',  ( -1.000000000000000000, -0.000000000000000000, 0.000000000000000000 ) ) ;
#6299 = ORIENTED_EDGE ( 'NONE', *, *, #2432, .F. ) ;
#6300 = LINE ( 'NONE', #2665, #4070 ) ;
#6301 = EDGE_CURVE ( 'NONE', #5674, #777, #8201, .T. ) ;
#6302 = DIRECTION ( 'NONE',  ( 0.000000000000000000, 0.000000000000000000, 1.000000000000000000 ) ) ;
#6303 = ORIENTED_EDGE ( 'NONE', *, *, #11251, .F. ) ;
#6304 = CARTESIAN_POINT ( 'NONE',  ( 46.00000000000000000, -3.499999999999998668, -45.49999999999998579 ) ) ;
#6305 = CIRCLE ( 'NONE', #4291, 9.600000000009602630 ) ;
#6306 = CARTESIAN_POINT ( 'NONE',  ( 4.999999999999999112, 0.000000000000000000, 0.000000000000000000 ) ) ;
#6307 = ORIENTED_EDGE ( 'NONE', *, *, #11709, .F. ) ;
#6308 = CARTESIAN_POINT ( 'NONE',  ( 4.999999999999999112, 0.000000000000000000, 0.000000000000000000 ) ) ;
#6309 = EDGE_CURVE ( 'NONE', #5984, #5745, #2380, .T. ) ;
#6310 = ORIENTED_EDGE ( 'NONE', *, *, #8084, .F. ) ;
#6311 = DIRECTION ( 'NONE',  ( 0.000000000000000000, 0.8660254037844398178, -0.4999999999999978906 ) ) ;
#6312 = ORIENTED_EDGE ( 'NONE', *, *, #6635, .T. ) ;
#6313 = EDGE_CURVE ( 'NONE', #9964, #1066, #834, .T. ) ;
#6314 = ADVANCED_FACE ( 'NONE', ( #10023 ), #2271, .T. ) ;
#6315 = DIRECTION ( 'NONE',  ( -1.000000000000000000, 0.000000000000000000, 0.000000000000000000 ) ) ;
#6316 = EDGE_LOOP ( 'NONE', ( #11077, #844, #5805, #10213, #8098, #9589, #1697, #11203 ) ) ;
#6317 = DIRECTION ( 'NONE',  ( 1.000000000000000000, 0.000000000000000000, 0.000000000000000000 ) ) ;
#6318 = CARTESIAN_POINT ( 'NONE',  ( 4.999999999999999112, 0.000000000000000000, 0.000000000000000000 ) ) ;
#6319 = CARTESIAN_POINT ( 'NONE',  ( 4.999999999999999112, 16.90755573046746107, -0.4834863907626340551 ) ) ;
#6320 = CARTESIAN_POINT ( 'NONE',  ( -20.63749999999999929, 0.000000000000000000, -5.000000000000000000 ) ) ;
#6321 = DIRECTION ( 'NONE',  ( 0.000000000000000000, 0.000000000000000000, 1.000000000000000000 ) ) ;
#6322 = VERTEX_POINT ( 'NONE', #6090 ) ;
#6323 = EDGE_LOOP ( 'NONE', ( #5635, #8311, #1537, #11840 ) ) ;
#6324 = DIRECTION ( 'NONE',  ( 0.000000000000000000, -0.9238795325112906243, 0.3826834323650805669 ) ) ;
#6325 = EDGE_CURVE ( 'NONE', #1905, #1094, #6838, .T. ) ;
#6326 = FILL_AREA_STYLE_COLOUR ( '', #1427 ) ;
#6327 = DIRECTION ( 'NONE',  ( 1.000000000000000000, 3.903127820947815962E-18, 0.000000000000000000 ) ) ;
#6328 = EDGE_CURVE ( 'NONE', #4999, #6297, #3214, .T. ) ;
#6329 = ORIENTED_EDGE ( 'NONE', *, *, #9232, .F. ) ;
#6330 = DIRECTION ( 'NONE',  ( -1.000000000000000000, 0.000000000000000000, 0.000000000000000000 ) ) ;
#6331 = VERTEX_POINT ( 'NONE', #6205 ) ;
#6332 = CARTESIAN_POINT ( 'NONE',  ( 6.080745460913608902, 0.5192545390863916310, 0.000000000000000000 ) ) ;
#6333 = LINE ( 'NONE', #2696, #8804 ) ;
#6334 = DIRECTION ( 'NONE',  ( 0.000000000000000000, 1.000000000000000000, -1.471414886128461471E-15 ) ) ;
#6335 = ADVANCED_FACE ( 'NONE', ( #4140 ), #5275, .T. ) ;
#6336 = ADVANCED_FACE ( 'NONE', ( #456 ), #3097, .T. ) ;
#6337 = CARTESIAN_POINT ( 'NONE',  ( 0.000000000000000000, -19.24938187143291657, -6.283573709965514453 ) ) ;
#6338 = LINE ( 'NONE', #8155, #4233 ) ;
#6339 = VERTEX_POINT ( 'NONE', #3334 ) ;
#6340 = DIRECTION ( 'NONE',  ( 0.000000000000000000, 0.000000000000000000, -1.000000000000000000 ) ) ;
#6341 = DIRECTION ( 'NONE',  ( 1.000000000000000000, 0.000000000000000000, 0.000000000000000000 ) ) ;
#6342 = ORIENTED_EDGE ( 'NONE', *, *, #7843, .F. ) ;
#6343 = CYLINDRICAL_SURFACE ( 'NONE', #7892, 9.600000000009600853 ) ;
#6344 = ORIENTED_EDGE ( 'NONE', *, *, #2537, .F. ) ;
#6345 = DIRECTION ( 'NONE',  ( 1.000000000000000000, 0.000000000000000000, 0.000000000000000000 ) ) ;
#6346 = CARTESIAN_POINT ( 'NONE',  ( 4.999999999999999112, 18.05452603534179090, -9.168210874537381372 ) ) ;
#6347 = DIRECTION ( 'NONE',  ( -1.000000000000000000, 4.770489558936235687E-18, -6.855277276495154548E-34 ) ) ;
#6348 = LINE ( 'NONE', #11278, #8633 ) ;
#6349 = DIRECTION ( 'NONE',  ( 0.000000000000000000, 0.000000000000000000, 1.000000000000000000 ) ) ;
#6350 = ORIENTED_EDGE ( 'NONE', *, *, #6986, .F. ) ;
#6351 = LINE ( 'NONE', #7172, #3253 ) ;
#6352 = VERTEX_POINT ( 'NONE', #3517 ) ;
#6353 = DIRECTION ( 'NONE',  ( 0.000000000000000000, 0.000000000000000000, 1.000000000000000000 ) ) ;
#6354 = CARTESIAN_POINT ( 'NONE',  ( 42.00000000000000000, 4.814824860968089633E-32, 0.000000000000000000 ) ) ;
#6355 = ORIENTED_EDGE ( 'NONE', *, *, #5482, .F. ) ;
#6356 = FACE_OUTER_BOUND ( 'NONE', #9351, .T. ) ;
#6357 = FACE_OUTER_BOUND ( 'NONE', #11602, .T. ) ;
#6358 = ORIENTED_EDGE ( 'NONE', *, *, #11430, .F. ) ;
#6359 = DIRECTION ( 'NONE',  ( -1.000000000000000000, 0.000000000000000000, 0.000000000000000000 ) ) ;
#6360 = VERTEX_POINT ( 'NONE', #7209 ) ;
#6361 = DIRECTION ( 'NONE',  ( -1.000000000000000000, -0.000000000000000000, -0.000000000000000000 ) ) ;
#6362 = ORIENTED_EDGE ( 'NONE', *, *, #5468, .T. ) ;
#6363 = AXIS2_PLACEMENT_3D ( 'NONE', #7125, #2355, #6121 ) ;
#6364 = CLOSED_SHELL ( 'NONE', ( #11110, #4625, #8884, #1414, #5371, #7538, #1552, #4025, #3059, #4334, #4958, #11135, #3416, #3121, #1418, #9601, #7076 ) ) ;
#6365 = DIRECTION ( 'NONE',  ( 0.000000000000000000, 0.000000000000000000, 1.000000000000000000 ) ) ;
#6366 = ORIENTED_EDGE ( 'NONE', *, *, #3796, .F. ) ;
#6367 = FACE_OUTER_BOUND ( 'NONE', #7025, .T. ) ;
#6368 = EDGE_CURVE ( 'NONE', #4096, #7260, #1843, .T. ) ;
#6369 = VECTOR ( 'NONE', #4348, 1000.000000000000000 ) ;
#6370 = CIRCLE ( 'NONE', #6786, 27.00000000002699707 ) ;
#6371 = DIRECTION ( 'NONE',  ( 0.000000000000000000, 0.000000000000000000, 1.000000000000000000 ) ) ;
#6372 = EDGE_CURVE ( 'NONE', #9803, #8928, #11930, .T. ) ;
#6373 = AXIS2_PLACEMENT_3D ( 'NONE', #4401, #526, #10961 ) ;
#6374 = DIRECTION ( 'NONE',  ( -0.000000000000000000, 0.000000000000000000, -1.000000000000000000 ) ) ;
#6375 = DIRECTION ( 'NONE',  ( -1.000000000000000000, -0.000000000000000000, -0.000000000000000000 ) ) ;
#6376 = DIRECTION ( 'NONE',  ( 0.000000000000000000, -0.000000000000000000, -1.000000000000000000 ) ) ;
#6377 = VERTEX_POINT ( 'NONE', #4378 ) ;
#6378 = EDGE_LOOP ( 'NONE', ( #6213, #8741 ) ) ;
#6379 = DIRECTION ( 'NONE',  ( -4.770489558936236458E-18, -1.000000000000000000, 0.000000000000000000 ) ) ;
#6380 =( NAMED_UNIT ( * ) SI_UNIT ( $, .STERADIAN. ) SOLID_ANGLE_UNIT ( ) );
#6381 = CARTESIAN_POINT ( 'NONE',  ( -10.00000000000000000, 0.000000000000000000, 0.000000000000000000 ) ) ;
#6382 = AXIS2_PLACEMENT_3D ( 'NONE', #4190, #8905, #7087 ) ;
#6383 = ORIENTED_EDGE ( 'NONE', *, *, #9722, .F. ) ;
#6384 = DIRECTION ( 'NONE',  ( -1.000000000000000000, -0.000000000000000000, -0.000000000000000000 ) ) ;
#6385 = VECTOR ( 'NONE', #3945, 1000.000000000000000 ) ;
#6386 = ORIENTED_EDGE ( 'NONE', *, *, #7106, .F. ) ;
#6387 = CARTESIAN_POINT ( 'NONE',  ( 4.999999999999999112, 15.22291137398942240, -14.46592441914948779 ) ) ;
#6388 = CIRCLE ( 'NONE', #994, 0.7500000000000000000 ) ;
#6389 = EDGE_CURVE ( 'NONE', #9911, #4914, #4630, .T. ) ;
#6390 = EDGE_CURVE ( 'NONE', #6028, #3139, #2630, .T. ) ;
#6391 = EDGE_CURVE ( 'NONE', #6545, #4760, #2561, .T. ) ;
#6392 = ADVANCED_FACE ( 'NONE', ( #5566 ), #7461, .F. ) ;
#6393 = AXIS2_PLACEMENT_3D ( 'NONE', #5868, #10726, #12342 ) ;
#6394 = CARTESIAN_POINT ( 'NONE',  ( 5.000000000000002665, 0.000000000000000000, -2.700000000000000622 ) ) ;
#6395 = DIRECTION ( 'NONE',  ( 0.000000000000000000, 0.000000000000000000, 1.000000000000000000 ) ) ;
#6396 = CIRCLE ( 'NONE', #2596, 27.00000000002699707 ) ;
#6397 = DIRECTION ( 'NONE',  ( 0.000000000000000000, 0.000000000000000000, 1.000000000000000000 ) ) ;
#6398 = CARTESIAN_POINT ( 'NONE',  ( 4.999999999999999112, 0.000000000000000000, 0.000000000000000000 ) ) ;
#6399 = EDGE_LOOP ( 'NONE', ( #10921, #4052, #9557, #11336 ) ) ;
#6400 = CARTESIAN_POINT ( 'NONE',  ( 0.000000000000000000, 0.000000000000000000, 0.000000000000000000 ) ) ;
#6401 = DIRECTION ( 'NONE',  ( 1.000000000000000000, -0.000000000000000000, -0.000000000000000000 ) ) ;
#6402 = ORIENTED_EDGE ( 'NONE', *, *, #3717, .F. ) ;
#6403 = CARTESIAN_POINT ( 'NONE',  ( 2.500000000000000000, 2.357898499370433054, -1.951563910473907981E-15 ) ) ;
#6404 = VERTEX_POINT ( 'NONE', #7283 ) ;
#6405 = AXIS2_PLACEMENT_3D ( 'NONE', #955, #207, #10712 ) ;
#6406 = EDGE_CURVE ( 'NONE', #5793, #10654, #9148, .T. ) ;
#6407 = VECTOR ( 'NONE', #8837, 1000.000000000000000 ) ;
#6408 = AXIS2_PLACEMENT_3D ( 'NONE', #1402, #226, #7165 ) ;
#6409 = PLANE ( 'NONE',  #9380 ) ;
#6410 = DIRECTION ( 'NONE',  ( 1.000000000000000000, -0.000000000000000000, 0.000000000000000000 ) ) ;
#6411 = CARTESIAN_POINT ( 'NONE',  ( 2.500000000000000444, -5.955107813822308138, -26.33508479058327367 ) ) ;
#6412 = DIRECTION ( 'NONE',  ( 1.000000000000000000, 0.000000000000000000, 0.000000000000000000 ) ) ;
#6413 = CARTESIAN_POINT ( 'NONE',  ( 25.00000000000000000, 0.000000000000000000, 0.000000000000000000 ) ) ;
#6414 = CIRCLE ( 'NONE', #3616, 2.041999999999999815 ) ;
#6415 = ORIENTED_EDGE ( 'NONE', *, *, #3207, .F. ) ;
#6416 = CIRCLE ( 'NONE', #8234, 5.000000000000004441 ) ;
#6417 = LINE ( 'NONE', #846, #3458 ) ;
#6418 = AXIS2_PLACEMENT_3D ( 'NONE', #9614, #9550, #11529 ) ;
#6419 = CIRCLE ( 'NONE', #1022, 9.600000000009600853 ) ;
#6420 = ORIENTED_EDGE ( 'NONE', *, *, #8089, .F. ) ;
#6421 = FILL_AREA_STYLE_COLOUR ( '', #6876 ) ;
#6422 = ORIENTED_EDGE ( 'NONE', *, *, #8029, .F. ) ;
#6423 = CARTESIAN_POINT ( 'NONE',  ( 4.999999999999999112, -9.168210874537708222, 18.05452603534162748 ) ) ;
#6424 = ADVANCED_FACE ( 'NONE', ( #12002 ), #11010, .T. ) ;
#6425 = CARTESIAN_POINT ( 'NONE',  ( 1.600000000000000089, 8.572527594031473190E-16, -7.000000000000000000 ) ) ;
#6426 =( GEOMETRIC_REPRESENTATION_CONTEXT ( 3 ) GLOBAL_UNCERTAINTY_ASSIGNED_CONTEXT ( ( #2025 ) ) GLOBAL_UNIT_ASSIGNED_CONTEXT ( ( #359, #10873, #2302 ) ) REPRESENTATION_CONTEXT ( 'NONE', 'WORKASPACE' ) );
#6427 = CIRCLE ( 'NONE', #2425, 27.00000000002699707 ) ;
#6428 = AXIS2_PLACEMENT_3D ( 'NONE', #5470, #11205, #2574 ) ;
#6429 = AXIS2_PLACEMENT_3D ( 'NONE', #7037, #11764, #3220 ) ;
#6430 = AXIS2_PLACEMENT_3D ( 'NONE', #1601, #3420, #5425 ) ;
#6431 = VERTEX_POINT ( 'NONE', #5330 ) ;
#6432 = DIRECTION ( 'NONE',  ( 0.000000000000000000, 1.000000000000000000, 3.373073425507084106E-15 ) ) ;
#6433 = VERTEX_POINT ( 'NONE', #562 ) ;
#6435 = CARTESIAN_POINT ( 'NONE',  ( 0.000000000000000000, 0.000000000000000000, 0.000000000000000000 ) ) ;
#6434 =( GEOMETRIC_REPRESENTATION_CONTEXT ( 3 ) GLOBAL_UNCERTAINTY_ASSIGNED_CONTEXT ( ( #5655 ) ) GLOBAL_UNIT_ASSIGNED_CONTEXT ( ( #8131, #2606, #9998 ) ) REPRESENTATION_CONTEXT ( 'NONE', 'WORKASPACE' ) );
#6436 = AXIS2_PLACEMENT_3D ( 'NONE', #1210, #3848, #4959 ) ;
#6437 = ORIENTED_EDGE ( 'NONE', *, *, #5956, .F. ) ;
#6438 = VECTOR ( 'NONE', #1631, 999.9999999999998863 ) ;
#6439 = VECTOR ( 'NONE', #9655, 1000.000000000000000 ) ;
#6440 = CARTESIAN_POINT ( 'NONE',  ( -1.399999999999999689, 9.062386313690412402E-16, 7.399999999999999467 ) ) ;
#6441 = VERTEX_POINT ( 'NONE', #6387 ) ;
#6442 = DIRECTION ( 'NONE',  ( 0.000000000000000000, -0.5000000000000072164, 0.8660254037844345998 ) ) ;
#6443 = PRODUCT_DEFINITION_FORMATION_WITH_SPECIFIED_SOURCE ( 'ANY', '', #9134, .NOT_KNOWN. ) ;
#6444 = VECTOR ( 'NONE', #3287, 1000.000000000000000 ) ;
#6445 = VECTOR ( 'NONE', #4694, 1000.000000000000000 ) ;
#6446 = CARTESIAN_POINT ( 'NONE',  ( 70.79898987322334847, -3.499999999999998668, -38.49999999999998579 ) ) ;
#6447 = VECTOR ( 'NONE', #3202, 1000.000000000000000 ) ;
#6448 = DIRECTION ( 'NONE',  ( 0.000000000000000000, 0.8772744497699203059, 0.4799891038147465760 ) ) ;
#6449 = CARTESIAN_POINT ( 'NONE',  ( 4.999999999999999112, 0.000000000000000000, 0.000000000000000000 ) ) ;
#6450 = VERTEX_POINT ( 'NONE', #2453 ) ;
#6451 = EDGE_LOOP ( 'NONE', ( #8309, #2775, #875, #11386 ) ) ;
#6452 = EDGE_CURVE ( 'NONE', #1992, #6028, #11131, .T. ) ;
#6453 = CARTESIAN_POINT ( 'NONE',  ( 4.999999999999999112, 5.950465759859149273, -20.13931372320382351 ) ) ;
#6454 =( LENGTH_UNIT ( ) NAMED_UNIT ( * ) SI_UNIT ( .MILLI., .METRE. ) );
#6455 = CARTESIAN_POINT ( 'NONE',  ( 37.00000000000000711, 4.817162211711309538, -40.66024322130446222 ) ) ;
#6456 = CIRCLE ( 'NONE', #10238, 25.00000000000000000 ) ;
#6457 = CARTESIAN_POINT ( 'NONE',  ( 0.000000000000000000, 0.000000000000000000, 0.000000000000000000 ) ) ;
#6458 = ADVANCED_FACE ( 'NONE', ( #8279 ), #6276, .F. ) ;
#6459 = VECTOR ( 'NONE', #5561, 1000.000000000000000 ) ;
#6460 = ORIENTED_EDGE ( 'NONE', *, *, #5099, .F. ) ;
#6461 = CARTESIAN_POINT ( 'NONE',  ( 2.499999999999999556, -22.83261415639492498, -14.41081992069334383 ) ) ;
#6462 = ADVANCED_BREP_SHAPE_REPRESENTATION ( '', ( #8531, #6056 ), #8443 ) ;
#6463 = DIRECTION ( 'NONE',  ( -1.000000000000000000, 0.000000000000000000, 0.000000000000000000 ) ) ;
#6464 = AXIS2_PLACEMENT_3D ( 'NONE', #4067, #9756, #8002 ) ;
#6465 = ORIENTED_EDGE ( 'NONE', *, *, #1520, .F. ) ;
#6466 = CARTESIAN_POINT ( 'NONE',  ( 25.00000000000000000, 6.123233995736766282E-16, -5.000000000000000000 ) ) ;
#6467 = DIRECTION ( 'NONE',  ( -1.000000000000000000, -0.000000000000000000, -0.000000000000000000 ) ) ;
#6468 = ORIENTED_EDGE ( 'NONE', *, *, #1734, .F. ) ;
#6469 = ADVANCED_FACE ( 'NONE', ( #10088 ), #5459, .T. ) ;
#6470 = CYLINDRICAL_SURFACE ( 'NONE', #6783, 25.00000000000000000 ) ;
#6471 = LINE ( 'NONE', #4463, #3027 ) ;
#6472 = ORIENTED_EDGE ( 'NONE', *, *, #10286, .F. ) ;
#6473 = DIRECTION ( 'NONE',  ( 1.000000000000000000, 0.000000000000000000, 0.000000000000000000 ) ) ;
#6474 = EDGE_CURVE ( 'NONE', #10654, #9690, #8329, .T. ) ;
#6475 = ORIENTED_EDGE ( 'NONE', *, *, #3660, .T. ) ;
#6476 = EDGE_CURVE ( 'NONE', #5665, #1460, #11971, .T. ) ;
#6477 = CIRCLE ( 'NONE', #8080, 4.799999999999998934 ) ;
#6478 = CARTESIAN_POINT ( 'NONE',  ( -20.00000000000000000, 40.00000000000000711, 12.50000000000000000 ) ) ;
#6479 = DIRECTION ( 'NONE',  ( -1.000000000000000000, -0.000000000000000000, -0.000000000000000000 ) ) ;
#6480 = DIRECTION ( 'NONE',  ( -1.000000000000000000, 0.000000000000000000, 0.000000000000000000 ) ) ;
#6481 = DIRECTION ( 'NONE',  ( -1.000000000000000000, -0.000000000000000000, -0.000000000000000000 ) ) ;
#6482 = CARTESIAN_POINT ( 'NONE',  ( 4.999999999999999112, 20.18872947935930995, -1.561154383803291967 ) ) ;
#6483 = ORIENTED_EDGE ( 'NONE', *, *, #9065, .F. ) ;
#6484 = ORIENTED_EDGE ( 'NONE', *, *, #5478, .F. ) ;
#6485 = AXIS2_PLACEMENT_3D ( 'NONE', #830, #12261, #1839 ) ;
#6486 = LINE ( 'NONE', #772, #852 ) ;
#6487 = ORIENTED_EDGE ( 'NONE', *, *, #4423, .T. ) ;
#6488 = CARTESIAN_POINT ( 'NONE',  ( 57.60000000000000142, 0.000000000000000000, -41.99999999999999289 ) ) ;
#6489 = ORIENTED_EDGE ( 'NONE', *, *, #1732, .F. ) ;
#6490 = PRODUCT_RELATED_PRODUCT_CATEGORY ( 'part', '', ( #9932 ) ) ;
#6491 = DIRECTION ( 'NONE',  ( 0.000000000000000000, 0.000000000000000000, -1.000000000000000000 ) ) ;
#6492 = PLANE ( 'NONE',  #3183 ) ;
#6493 = AXIS2_PLACEMENT_3D ( 'NONE', #5749, #7457, #5697 ) ;
#6494 = ORIENTED_EDGE ( 'NONE', *, *, #324, .F. ) ;
#6495 = DIRECTION ( 'NONE',  ( -1.000000000000000000, 0.000000000000000000, 0.000000000000000000 ) ) ;
#6496 = DIRECTION ( 'NONE',  ( -1.000000000000000000, -0.000000000000000000, -0.000000000000000000 ) ) ;
#6497 = VERTEX_POINT ( 'NONE', #6332 ) ;
#6498 = EDGE_CURVE ( 'NONE', #8156, #7335, #9211, .T. ) ;
#6499 = ADVANCED_FACE ( 'NONE', ( #748 ), #12182, .T. ) ;
#6500 = LINE ( 'NONE', #3550, #8978 ) ;
#6501 = VERTEX_POINT ( 'NONE', #7649 ) ;
#6502 = AXIS2_PLACEMENT_3D ( 'NONE', #2627, #509, #8277 ) ;
#6503 = LINE ( 'NONE', #12294, #12074 ) ;
#6504 = EDGE_LOOP ( 'NONE', ( #52, #6589, #7569, #8697 ) ) ;
#6505 = CYLINDRICAL_SURFACE ( 'NONE', #3363, 7.200000000007202416 ) ;
#6506 = DIRECTION ( 'NONE',  ( -1.000000000000000000, -0.000000000000000000, 0.000000000000000000 ) ) ;
#6507 = CARTESIAN_POINT ( 'NONE',  ( 0.000000000000000000, -8.527191590521155717, 11.41582255376070343 ) ) ;
#6508 = DIRECTION ( 'NONE',  ( -1.000000000000000000, 0.000000000000000000, -0.000000000000000000 ) ) ;
#6509 = ORIENTED_EDGE ( 'NONE', *, *, #11100, .F. ) ;
#6510 = ORIENTED_EDGE ( 'NONE', *, *, #11271, .F. ) ;
#6511 = CARTESIAN_POINT ( 'NONE',  ( 50.00005079999999680, 4.769696007084728073, -1.500000000000000000 ) ) ;
#6512 = DIRECTION ( 'NONE',  ( -1.000000000000000000, 0.000000000000000000, 0.000000000000000000 ) ) ;
#6513 = CARTESIAN_POINT ( 'NONE',  ( 0.000000000000000000, 2.357898499370433054, -1.951563910473907981E-15 ) ) ;
#6514 = ORIENTED_EDGE ( 'NONE', *, *, #4924, .T. ) ;
#6515 = DIRECTION ( 'NONE',  ( 0.000000000000000000, 0.000000000000000000, 1.000000000000000000 ) ) ;
#6516 = PRODUCT ( 'plain washer 10669 type nl_iso_ISO 10669-5.4-N', 'plain washer 10669 type nl_iso_ISO 10669-5.4-N', '', ( #8487 ) ) ;
#6517 = LINE ( 'NONE', #5461, #1808 ) ;
#6518 = CARTESIAN_POINT ( 'NONE',  ( 36.00000000000000000, 40.00000000000000711, 20.00000000000001066 ) ) ;
#6519 = EDGE_CURVE ( 'NONE', #11243, #4159, #9837, .T. ) ;
#6520 = ORIENTED_EDGE ( 'NONE', *, *, #6166, .T. ) ;
#6521 = CARTESIAN_POINT ( 'NONE',  ( 1.400000000000000133, 0.000000000000000000, -5.100000000000000533 ) ) ;
#6522 = CARTESIAN_POINT ( 'NONE',  ( 0.000000000000000000, 14.40062958310465469, 8.872489362018239234 ) ) ;
#6523 = EDGE_LOOP ( 'NONE', ( #6134, #6948, #5324, #6152 ) ) ;
#6524 = FACE_OUTER_BOUND ( 'NONE', #111, .T. ) ;
#6525 = CYLINDRICAL_SURFACE ( 'NONE', #5818, 7.200000000007202416 ) ;
#6526 = EDGE_LOOP ( 'NONE', ( #8488, #10036, #6934, #3885 ) ) ;
#6527 = DIRECTION ( 'NONE',  ( -1.000000000000000000, 0.000000000000000000, -0.000000000000000000 ) ) ;
#6528 = ORIENTED_EDGE ( 'NONE', *, *, #2740, .F. ) ;
#6529 = EDGE_CURVE ( 'NONE', #7347, #9806, #8576, .T. ) ;
#6530 = CARTESIAN_POINT ( 'NONE',  ( 0.000000000000000000, 0.5192545390863916310, -1.000000000000000000 ) ) ;
#6531 = LINE ( 'NONE', #9167, #12185 ) ;
#6532 = ADVANCED_FACE ( 'NONE', ( #4820 ), #1820, .F. ) ;
#6533 = FACE_OUTER_BOUND ( 'NONE', #10177, .T. ) ;
#6534 = DIRECTION ( 'NONE',  ( -1.000000000000000000, -0.000000000000000000, -0.000000000000000000 ) ) ;
#6535 = ORIENTED_EDGE ( 'NONE', *, *, #11079, .T. ) ;
#6536 = EDGE_LOOP ( 'NONE', ( #12191, #10087, #604, #10107 ) ) ;
#6537 = DIRECTION ( 'NONE',  ( 0.000000000000000000, -0.8660254037844433705, 0.4999999999999920064 ) ) ;
#6538 = VERTEX_POINT ( 'NONE', #941 ) ;
#6539 = DIRECTION ( 'NONE',  ( 0.000000000000000000, 0.000000000000000000, -1.000000000000000000 ) ) ;
#6540 = SHAPE_DEFINITION_REPRESENTATION ( #8724, #1953 ) ;
#6541 = ORIENTED_EDGE ( 'NONE', *, *, #6933, .F. ) ;
#6542 = CARTESIAN_POINT ( 'NONE',  ( -36.00000000000000000, 0.000000000000000000, 0.000000000000000000 ) ) ;
#6543 = DIRECTION ( 'NONE',  ( -1.000000000000000000, 0.000000000000000000, 0.000000000000000000 ) ) ;
#6544 = ORIENTED_EDGE ( 'NONE', *, *, #10179, .T. ) ;
#6545 = VERTEX_POINT ( 'NONE', #4754 ) ;
#6546 = CARTESIAN_POINT ( 'NONE',  ( 1.000000000000000000, 0.5999999999999998668, 3.826895796574397046 ) ) ;
#6547 = EDGE_CURVE ( 'NONE', #5359, #8297, #9239, .T. ) ;
#6548 = EDGE_CURVE ( 'NONE', #7872, #4612, #7761, .T. ) ;
#6549 = DIRECTION ( 'NONE',  ( -1.000000000000000000, -0.000000000000000000, -0.000000000000000000 ) ) ;
#6550 = ADVANCED_FACE ( 'NONE', ( #77, #11552 ), #8644, .T. ) ;
#6551 = VERTEX_POINT ( 'NONE', #3701 ) ;
#6552 = CARTESIAN_POINT ( 'NONE',  ( 36.00000000000000711, 0.000000000000000000, 0.000000000000000000 ) ) ;
#6553 = ORIENTED_EDGE ( 'NONE', *, *, #10193, .F. ) ;
#6554 = CARTESIAN_POINT ( 'NONE',  ( 5.000000000000000000, 0.000000000000000000, 0.000000000000000000 ) ) ;
#6555 = ORIENTED_EDGE ( 'NONE', *, *, #1100, .T. ) ;
#6556 = LINE ( 'NONE', #3745, #7370 ) ;
#6557 = EDGE_CURVE ( 'NONE', #1857, #3502, #11373, .T. ) ;
#6558 = ADVANCED_FACE ( 'NONE', ( #7713 ), #2580, .T. ) ;
#6559 = DIRECTION ( 'NONE',  ( 1.000000000000000000, 0.000000000000000000, 0.000000000000000000 ) ) ;
#6560 = TOROIDAL_SURFACE ( 'NONE', #9775, 5.100000000000000533, 0.1000000000000001582 ) ;
#6561 = CIRCLE ( 'NONE', #2563, 7.200000000007202416 ) ;
#6562 = CIRCLE ( 'NONE', #4963, 40.00000000000000711 ) ;
#6563 = DIRECTION ( 'NONE',  ( -1.000000000000000000, 0.000000000000000000, 0.000000000000000000 ) ) ;
#6564 = CARTESIAN_POINT ( 'NONE',  ( 0.000000000000000000, -15.57980286237488343, 22.05152472667124997 ) ) ;
#6565 = ORIENTED_EDGE ( 'NONE', *, *, #1804, .F. ) ;
#6566 = ORIENTED_EDGE ( 'NONE', *, *, #5870, .T. ) ;
#6567 = CARTESIAN_POINT ( 'NONE',  ( 4.999999999999999112, -16.90755573046745752, 6.716513609244448624 ) ) ;
#6568 = SHAPE_REPRESENTATION_RELATIONSHIP ( 'NONE' , 'NONE' ,  #11360, #7062 ) ;
#6569 = DIRECTION ( 'NONE',  ( 0.000000000000000000, 0.8772744497699203059, 0.4799891038147465760 ) ) ;
#6570 = CARTESIAN_POINT ( 'NONE',  ( 4.999999999999999112, -5.984728032764810024, -21.74405275335764287 ) ) ;
#6571 = EDGE_LOOP ( 'NONE', ( #12196, #10172 ) ) ;
#6572 = CARTESIAN_POINT ( 'NONE',  ( 37.00000000000000711, 1.456773409934505593E-31, -41.99999999999998579 ) ) ;
#6573 = AXIS2_PLACEMENT_3D ( 'NONE', #3310, #7121, #6173 ) ;
#6574 = CIRCLE ( 'NONE', #10766, 40.00000000000000711 ) ;
#6575 = EDGE_CURVE ( 'NONE', #2734, #11589, #10565, .T. ) ;
#6576 = CARTESIAN_POINT ( 'NONE',  ( 0.000000000000000000, 0.000000000000000000, 1.500000000000000000 ) ) ;
#6577 = DIRECTION ( 'NONE',  ( 0.000000000000000000, 0.000000000000000000, 1.000000000000000000 ) ) ;
#6578 = ORIENTED_EDGE ( 'NONE', *, *, #7079, .F. ) ;
#6579 = DIRECTION ( 'NONE',  ( -1.000000000000000000, -0.000000000000000000, -0.000000000000000000 ) ) ;
#6580 = PLANE ( 'NONE',  #2846 ) ;
#6581 = AXIS2_PLACEMENT_3D ( 'NONE', #5012, #3277, #7771 ) ;
#6582 = AXIS2_PLACEMENT_3D ( 'NONE', #10506, #12352, #6712 ) ;
#6583 = EDGE_LOOP ( 'NONE', ( #3302, #2159 ) ) ;
#6584 = DIRECTION ( 'NONE',  ( -0.000000000000000000, 1.000000000000000000, -0.000000000000000000 ) ) ;
#6585 = DIRECTION ( 'NONE',  ( 0.000000000000000000, 0.000000000000000000, -1.000000000000000000 ) ) ;
#6586 = AXIS2_PLACEMENT_3D ( 'NONE', #3592, #11953, #11212 ) ;
#6587 = ORIENTED_EDGE ( 'NONE', *, *, #9515, .T. ) ;
#6588 = DIRECTION ( 'NONE',  ( -1.000000000000000000, -0.000000000000000000, -0.000000000000000000 ) ) ;
#6589 = ORIENTED_EDGE ( 'NONE', *, *, #1112, .T. ) ;
#6590 = VECTOR ( 'NONE', #3166, 1000.000000000000000 ) ;
#6591 = FILL_AREA_STYLE ('',( #11325 ) ) ;
#6592 = AXIS2_PLACEMENT_3D ( 'NONE', #2308, #6128, #7010 ) ;
#6593 = FACE_OUTER_BOUND ( 'NONE', #5595, .T. ) ;
#6594 = CARTESIAN_POINT ( 'NONE',  ( -36.00000000000000711, 0.000000000000000000, 40.00000000000000711 ) ) ;
#6595 = CARTESIAN_POINT ( 'NONE',  ( 0.1920286436967153787, 0.000000000000000000, 0.000000000000000000 ) ) ;
#6596 = CARTESIAN_POINT ( 'NONE',  ( 5.000000000000004441, 0.000000000000000000, 0.000000000000000000 ) ) ;
#6597 = VERTEX_POINT ( 'NONE', #7516 ) ;
#6598 = ORIENTED_EDGE ( 'NONE', *, *, #10283, .T. ) ;
#6599 = DIRECTION ( 'NONE',  ( 1.000000000000000000, 0.000000000000000000, 0.000000000000000000 ) ) ;
#6600 = AXIS2_PLACEMENT_3D ( 'NONE', #8593, #3100, #7671 ) ;
#6601 = ORIENTED_EDGE ( 'NONE', *, *, #414, .F. ) ;
#6602 = CARTESIAN_POINT ( 'NONE',  ( 15.00000000000000355, 40.00000000000000711, 0.000000000000000000 ) ) ;
#6603 = ADVANCED_FACE ( 'NONE', ( #2010 ), #2750, .F. ) ;
#6604 = DIRECTION ( 'NONE',  ( 0.000000000000000000, 0.000000000000000000, 1.000000000000000000 ) ) ;
#6605 = VECTOR ( 'NONE', #3673, 1000.000000000000000 ) ;
#6606 = ORIENTED_EDGE ( 'NONE', *, *, #5750, .F. ) ;
#6607 = VECTOR ( 'NONE', #1999, 1000.000000000000000 ) ;
#6608 = DIRECTION ( 'NONE',  ( 1.000000000000000000, 0.000000000000000000, 0.000000000000000000 ) ) ;
#6609 = EDGE_CURVE ( 'NONE', #5264, #720, #882, .T. ) ;
#6610 = CARTESIAN_POINT ( 'NONE',  ( 0.000000000000000000, 14.41081992069341133, -22.83261415639488234 ) ) ;
#6611 = ORIENTED_EDGE ( 'NONE', *, *, #6728, .T. ) ;
#6612 = CIRCLE ( 'NONE', #8820, 5.199999999999996625 ) ;
#6613 = VERTEX_POINT ( 'NONE', #8706 ) ;
#6614 = FACE_OUTER_BOUND ( 'NONE', #3957, .T. ) ;
#6615 = ADVANCED_BREP_SHAPE_REPRESENTATION ( '', ( #8493, #6056 ), #6434 ) ;
#6616 = AXIS2_PLACEMENT_3D ( 'NONE', #10964, #6978, #4153 ) ;
#6617 = CARTESIAN_POINT ( 'NONE',  ( 26.00000000000000355, 0.000000000000000000, 0.000000000000000000 ) ) ;
#6618 = CARTESIAN_POINT ( 'NONE',  ( 2.499999999999998668, 5.950465759858869497, 20.13931372320390523 ) ) ;
#6619 = ORIENTED_EDGE ( 'NONE', *, *, #3902, .T. ) ;
#6620 = DIRECTION ( 'NONE',  ( 0.000000000000000000, 0.000000000000000000, -1.000000000000000000 ) ) ;
#6621 = EDGE_LOOP ( 'NONE', ( #11128, #3114, #9914, #9467 ) ) ;
#6622 = ADVANCED_FACE ( 'NONE', ( #11444 ), #4698, .T. ) ;
#6623 = ORIENTED_EDGE ( 'NONE', *, *, #1294, .F. ) ;
#6624 = AXIS2_PLACEMENT_3D ( 'NONE', #4476, #3725, #8298 ) ;
#6625 = VECTOR ( 'NONE', #4047, 1000.000000000000114 ) ;
#6626 = DIRECTION ( 'NONE',  ( 0.000000000000000000, 0.000000000000000000, -1.000000000000000000 ) ) ;
#6627 = VECTOR ( 'NONE', #5208, 1000.000000000000114 ) ;
#6628 = PRODUCT ( 'spur gear_iso_ISO - Spur gear 3M 16T 20PA 5FW ---S16A75H50L10.0S1', 'spur gear_iso_ISO - Spur gear 3M 16T 20PA 5FW ---S16A75H50L10.0S1', '', ( #3728 ) ) ;
#6629 = EDGE_CURVE ( 'NONE', #1320, #1424, #8518, .T. ) ;
#6630 = CIRCLE ( 'NONE', #3618, 7.200000000007203305 ) ;
#6632 = VERTEX_POINT ( 'NONE', #812 ) ;
#6631 = ADVANCED_FACE ( 'NONE', ( #6650 ), #10640, .F. ) ;
#6633 = DIRECTION ( 'NONE',  ( 1.000000000000000000, -0.000000000000000000, -0.000000000000000000 ) ) ;
#6634 = CIRCLE ( 'NONE', #7827, 5.000000000000000000 ) ;
#6635 = EDGE_CURVE ( 'NONE', #5665, #11480, #1971, .T. ) ;
#6636 = LINE ( 'NONE', #3882, #4002 ) ;
#6637 = COLOUR_RGB ( '',0.8941176470588234615, 0.8941176470588234615, 0.8941176470588234615 ) ;
#6638 = AXIS2_PLACEMENT_3D ( 'NONE', #3721, #7534, #4472 ) ;
#6639 = VECTOR ( 'NONE', #1563, 1000.000000000000000 ) ;
#6640 = AXIS2_PLACEMENT_3D ( 'NONE', #12324, #3778, #7597 ) ;
#6641 = AXIS2_PLACEMENT_3D ( 'NONE', #4317, #1754, #7393 ) ;
#6642 = DIRECTION ( 'NONE',  ( 0.000000000000000000, 0.000000000000000000, -1.000000000000000000 ) ) ;
#6643 = CARTESIAN_POINT ( 'NONE',  ( 4.999999999999999112, 5.622796541391749336, -13.09267581720861173 ) ) ;
#6644 = ORIENTED_EDGE ( 'NONE', *, *, #3771, .F. ) ;
#6645 = EDGE_LOOP ( 'NONE', ( #11341, #1349 ) ) ;
#6646 = DIRECTION ( 'NONE',  ( 0.000000000000000000, 0.000000000000000000, 1.000000000000000000 ) ) ;
#6647 = DIRECTION ( 'NONE',  ( 0.000000000000000000, -1.224646799147352961E-16, 1.000000000000000000 ) ) ;
#6648 = DIRECTION ( 'NONE',  ( -1.000000000000000000, 0.000000000000000000, -0.000000000000000000 ) ) ;
#6649 = EDGE_LOOP ( 'NONE', ( #3239, #2111, #5064, #5471 ) ) ;
#6650 = FACE_OUTER_BOUND ( 'NONE', #4981, .T. ) ;
#6651 = PRESENTATION_LAYER_ASSIGNMENT (  '', '', ( #5039 ) ) ;
#6652 = CIRCLE ( 'NONE', #1241, 5.000000000000000000 ) ;
#6653 = AXIS2_PLACEMENT_3D ( 'NONE', #5893, #9645, #1071 ) ;
#6654 = AXIS2_PLACEMENT_3D ( 'NONE', #3523, #8282, #7342 ) ;
#6655 = CARTESIAN_POINT ( 'NONE',  ( 4.999999999999999112, -19.24938187143291657, -6.283573709965514453 ) ) ;
#6656 = CARTESIAN_POINT ( 'NONE',  ( 0.000000000000000000, -1.178949249685213863, 2.042000000000002924 ) ) ;
#6657 = DIRECTION ( 'NONE',  ( 1.000000000000000000, 0.000000000000000000, -0.000000000000000000 ) ) ;
#6658 = AXIS2_PLACEMENT_3D ( 'NONE', #3089, #2133, #11447 ) ;
#6659 = ORIENTED_EDGE ( 'NONE', *, *, #9595, .F. ) ;
#6660 = DIRECTION ( 'NONE',  ( -1.000000000000000000, -0.000000000000000000, -0.000000000000000000 ) ) ;
#6661 = EDGE_CURVE ( 'NONE', #10913, #5352, #4151, .T. ) ;
#6662 = FACE_OUTER_BOUND ( 'NONE', #2899, .T. ) ;
#6663 = EDGE_CURVE ( 'NONE', #3666, #344, #8760, .T. ) ;
#6664 = VERTEX_POINT ( 'NONE', #5000 ) ;
#6665 = DIRECTION ( 'NONE',  ( -1.000000000000000000, -0.000000000000000000, -0.000000000000000000 ) ) ;
#6666 = UNCERTAINTY_MEASURE_WITH_UNIT (LENGTH_MEASURE( 1.000000000000000082E-05 ), #3804, 'distance_accuracy_value', 'NONE');
#6667 = VERTEX_POINT ( 'NONE', #364 ) ;
#6668 = DIRECTION ( 'NONE',  ( 0.000000000000000000, -0.000000000000000000, -1.000000000000000000 ) ) ;
#6669 =( REPRESENTATION_RELATIONSHIP ('NONE','NONE', #9709, #1544 ) REPRESENTATION_RELATIONSHIP_WITH_TRANSFORMATION ( #7158 )SHAPE_REPRESENTATION_RELATIONSHIP( ) );
#6670 = LINE ( 'NONE', #9593, #9392 ) ;
#6671 = DIRECTION ( 'NONE',  ( -1.000000000000000000, 0.000000000000000000, 0.000000000000000000 ) ) ;
#6672 = DIRECTION ( 'NONE',  ( -1.000000000000000000, 0.000000000000000000, -0.000000000000000000 ) ) ;
#6673 = CARTESIAN_POINT ( 'NONE',  ( 1.095413108702814053, 0.000000000000000000, 0.000000000000000000 ) ) ;
#6674 = ORIENTED_EDGE ( 'NONE', *, *, #10283, .F. ) ;
#6675 = ORIENTED_EDGE ( 'NONE', *, *, #4167, .T. ) ;
#6676 = DIRECTION ( 'NONE',  ( 0.000000000000000000, 0.000000000000000000, 1.000000000000000000 ) ) ;
#6677 = ORIENTED_EDGE ( 'NONE', *, *, #10995, .F. ) ;
#6678 =( NAMED_UNIT ( * ) PLANE_ANGLE_UNIT ( ) SI_UNIT ( $, .RADIAN. ) );
#6679 = APPLICATION_PROTOCOL_DEFINITION ( 'draft international standard', 'automotive_design', 1998, #11353 ) ;
#6680 = CIRCLE ( 'NONE', #5268, 4.799999999999999822 ) ;
#6681 = ORIENTED_EDGE ( 'NONE', *, *, #9355, .F. ) ;
#6682 = CARTESIAN_POINT ( 'NONE',  ( 65.79898987322334847, -7.000000000000004441, -41.99999999999998579 ) ) ;
#6683 = DIRECTION ( 'NONE',  ( 0.000000000000000000, 1.000000000000000000, 0.000000000000000000 ) ) ;
#6684 = VERTEX_POINT ( 'NONE', #7896 ) ;
#6685 = ORIENTED_EDGE ( 'NONE', *, *, #12127, .T. ) ;
#6686 = CARTESIAN_POINT ( 'NONE',  ( 2.399999999999999467, 2.449293598294706414E-16, -2.000000000000000000 ) ) ;
#6687 = DIRECTION ( 'NONE',  ( 0.9914448613738102711, -0.1305261922200524338, 0.000000000000000000 ) ) ;
#6688 = AXIS2_PLACEMENT_3D ( 'NONE', #7603, #6793, #7679 ) ;
#6689 = DIRECTION ( 'NONE',  ( 0.000000000000000000, -6.982962677686266711E-15, 1.000000000000000000 ) ) ;
#6690 = DIRECTION ( 'NONE',  ( 1.000000000000000000, -0.000000000000000000, -0.000000000000000000 ) ) ;
#6691 = EDGE_CURVE ( 'NONE', #7692, #5247, #8082, .T. ) ;
#6692 = ORIENTED_EDGE ( 'NONE', *, *, #285, .F. ) ;
#6693 = CARTESIAN_POINT ( 'NONE',  ( 4.999999999999999112, 16.90755573046746107, -0.4834863907626340551 ) ) ;
#6694 = EDGE_LOOP ( 'NONE', ( #6475, #7559 ) ) ;
#6695 = ORIENTED_EDGE ( 'NONE', *, *, #3117, .T. ) ;
#6696 = CARTESIAN_POINT ( 'NONE',  ( -10.00000000000000000, 0.000000000000000000, 0.000000000000000000 ) ) ;
#6697 = CIRCLE ( 'NONE', #3098, 9.600000000009600853 ) ;
#6698 = EDGE_LOOP ( 'NONE', ( #7983, #5856, #11056, #917 ) ) ;
#6699 = DIRECTION ( 'NONE',  ( 0.000000000000000000, 0.000000000000000000, -1.000000000000000000 ) ) ;
#6700 = CARTESIAN_POINT ( 'NONE',  ( -7.839872433920653082E-18, 0.000000000000000000, 0.000000000000000000 ) ) ;
#6701 = EDGE_CURVE ( 'NONE', #6441, #5917, #8182, .T. ) ;
#6702 = EDGE_CURVE ( 'NONE', #2147, #11069, #3085, .T. ) ;
#6703 = VECTOR ( 'NONE', #3082, 1000.000000000000000 ) ;
#6704 = CARTESIAN_POINT ( 'NONE',  ( 50.00005079999999680, 6.799999999999999822, 1.500000000000000000 ) ) ;
#6705 = DIRECTION ( 'NONE',  ( -1.000000000000000000, -0.000000000000000000, -0.000000000000000000 ) ) ;
#6706 = ADVANCED_FACE ( 'NONE', ( #186 ), #1252, .T. ) ;
#6707 = EDGE_LOOP ( 'NONE', ( #11890, #8973, #2463, #5808 ) ) ;
#6708 = CARTESIAN_POINT ( 'NONE',  ( 42.00000000000000000, -3.792354139917828881, -2.942456469932581253 ) ) ;
#6709 = DIRECTION ( 'NONE',  ( 0.000000000000000000, 0.000000000000000000, -1.000000000000000000 ) ) ;
#6710 = FACE_OUTER_BOUND ( 'NONE', #10314, .T. ) ;
#6711 = ORIENTED_EDGE ( 'NONE', *, *, #11864, .T. ) ;
#6712 = DIRECTION ( 'NONE',  ( -0.000000000000000000, 0.000000000000000000, 1.000000000000000000 ) ) ;
#6713 = VECTOR ( 'NONE', #9319, 1000.000000000000000 ) ;
#6714 = CARTESIAN_POINT ( 'NONE',  ( 1.400000000000001910, 0.000000000000000000, 0.000000000000000000 ) ) ;
#6715 = CARTESIAN_POINT ( 'NONE',  ( 4.999999999999999112, 0.000000000000000000, 0.000000000000000000 ) ) ;
#6716 = EDGE_CURVE ( 'NONE', #3733, #11755, #10927, .T. ) ;
#6717 = EDGE_CURVE ( 'NONE', #10764, #1709, #1363, .T. ) ;
#6718 = CARTESIAN_POINT ( 'NONE',  ( 14.39999999999999680, 0.000000000000000000, 0.000000000000000000 ) ) ;
#6719 = DIRECTION ( 'NONE',  ( 0.9961946980917455452, 0.000000000000000000, -0.08715574274765813811 ) ) ;
#6720 = ADVANCED_FACE ( 'NONE', ( #7948 ), #6126, .T. ) ;
#6721 = ORIENTED_EDGE ( 'NONE', *, *, #6794, .F. ) ;
#6722 = CARTESIAN_POINT ( 'NONE',  ( 4.999999999999999112, -18.05452603534159195, -9.168210874537770394 ) ) ;
#6723 = DIRECTION ( 'NONE',  ( 0.000000000000000000, 0.7071067811865487940, -0.7071067811865462405 ) ) ;
#6724 = ORIENTED_EDGE ( 'NONE', *, *, #12236, .F. ) ;
#6725 = DIRECTION ( 'NONE',  ( 0.000000000000000000, -9.486769009248163798E-17, 1.000000000000000000 ) ) ;
#6726 = ORIENTED_EDGE ( 'NONE', *, *, #2505, .T. ) ;
#6727 = EDGE_CURVE ( 'NONE', #811, #3527, #312, .T. ) ;
#6728 = EDGE_CURVE ( 'NONE', #2318, #811, #7795, .T. ) ;
#6729 = DIRECTION ( 'NONE',  ( -1.000000000000000000, 4.770489558936236458E-18, -6.855277276495154548E-34 ) ) ;
#6730 = FACE_BOUND ( 'NONE', #6809, .T. ) ;
#6731 = DIRECTION ( 'NONE',  ( 0.03086419753086420623, -0.9995235871707959241, 0.000000000000000000 ) ) ;
#6732 = DIRECTION ( 'NONE',  ( -1.000000000000000000, 0.000000000000000000, 0.000000000000000000 ) ) ;
#6733 = ORIENTED_EDGE ( 'NONE', *, *, #10447, .F. ) ;
#6734 = VERTEX_POINT ( 'NONE', #2362 ) ;
#6735 = DIRECTION ( 'NONE',  ( 0.000000000000000000, 0.000000000000000000, 1.000000000000000000 ) ) ;
#6736 = ORIENTED_EDGE ( 'NONE', *, *, #5770, .T. ) ;
#6737 = CYLINDRICAL_SURFACE ( 'NONE', #8476, 14.24900000001425227 ) ;
#6738 = CONTEXT_DEPENDENT_SHAPE_REPRESENTATION ( #8577, #10035 ) ;
#6739 = ORIENTED_EDGE ( 'NONE', *, *, #5267, .F. ) ;
#6740 = EDGE_LOOP ( 'NONE', ( #6879, #7057, #8943, #5122 ) ) ;
#6741 = ORIENTED_EDGE ( 'NONE', *, *, #5934, .T. ) ;
#6742 = CARTESIAN_POINT ( 'NONE',  ( -10.00000000000000000, 0.000000000000000000, 0.000000000000000000 ) ) ;
#6743 = LINE ( 'NONE', #5732, #9813 ) ;
#6744 = LINE ( 'NONE', #10610, #6625 ) ;
#6745 = CARTESIAN_POINT ( 'NONE',  ( 0.000000000000000000, -19.60720892790260805, 11.14352537685167732 ) ) ;
#6746 = ORIENTED_EDGE ( 'NONE', *, *, #6813, .T. ) ;
#6747 = DIRECTION ( 'NONE',  ( 0.000000000000000000, 0.000000000000000000, -1.000000000000000000 ) ) ;
#6748 = ORIENTED_EDGE ( 'NONE', *, *, #2634, .F. ) ;
#6749 = VERTEX_POINT ( 'NONE', #6074 ) ;
#6750 = CARTESIAN_POINT ( 'NONE',  ( 1.600000000000000089, 0.000000000000000000, 0.000000000000000000 ) ) ;
#6751 = ORIENTED_EDGE ( 'NONE', *, *, #9556, .T. ) ;
#6752 = CARTESIAN_POINT ( 'NONE',  ( 4.999999999999999112, -19.60720892790245529, -11.14352537685195266 ) ) ;
#6753 = DIRECTION ( 'NONE',  ( 0.000000000000000000, 0.000000000000000000, 1.000000000000000000 ) ) ;
#6754 = CARTESIAN_POINT ( 'NONE',  ( 0.000000000000000000, -0.6000000000000000888, 2.622672778259560467 ) ) ;
#6755 = DIRECTION ( 'NONE',  ( 1.000000000000000000, -0.000000000000000000, -0.000000000000000000 ) ) ;
#6756 = VERTEX_POINT ( 'NONE', #11737 ) ;
#6757 = CARTESIAN_POINT ( 'NONE',  ( -36.00000000000000000, 0.000000000000000000, 0.000000000000000000 ) ) ;
#6758 = DIRECTION ( 'NONE',  ( -1.000000000000000000, 0.000000000000000000, 0.000000000000000000 ) ) ;
#6759 = FACE_OUTER_BOUND ( 'NONE', #8669, .T. ) ;
#6760 = EDGE_CURVE ( 'NONE', #420, #3401, #386, .T. ) ;
#6761 = ORIENTED_EDGE ( 'NONE', *, *, #6858, .F. ) ;
#6762 = CARTESIAN_POINT ( 'NONE',  ( 4.999999999999999112, 11.41582255376084909, -8.527191590520953213 ) ) ;
#6763 = ADVANCED_FACE ( 'NONE', ( #1184 ), #4249, .T. ) ;
#6764 = AXIS2_PLACEMENT_3D ( 'NONE', #726, #7179, #10167 ) ;
#6765 = CIRCLE ( 'NONE', #8763, 2.149999999999999023 ) ;
#6766 =( NAMED_UNIT ( * ) PLANE_ANGLE_UNIT ( ) SI_UNIT ( $, .RADIAN. ) );
#6767 = DIRECTION ( 'NONE',  ( 0.000000000000000000, 0.000000000000000000, 1.000000000000000000 ) ) ;
#6768 = DIRECTION ( 'NONE',  ( 1.000000000000000000, 0.000000000000000000, 0.000000000000000000 ) ) ;
#6769 = PLANE ( 'NONE',  #1639 ) ;
#6770 = ORIENTED_EDGE ( 'NONE', *, *, #10152, .T. ) ;
#6771 = FACE_OUTER_BOUND ( 'NONE', #5517, .T. ) ;
#6772 = DIRECTION ( 'NONE',  ( 0.000000000000000000, 0.000000000000000000, -1.000000000000000000 ) ) ;
#6773 = CIRCLE ( 'NONE', #4968, 7.500000000000000888 ) ;
#6774 = ORIENTED_EDGE ( 'NONE', *, *, #3356, .F. ) ;
#6775 = FACE_OUTER_BOUND ( 'NONE', #2473, .T. ) ;
#6776 = UNCERTAINTY_MEASURE_WITH_UNIT (LENGTH_MEASURE( 1.000000000000000082E-05 ), #636, 'distance_accuracy_value', 'NONE');
#6777 = CIRCLE ( 'NONE', #4163, 5.000000000000000000 ) ;
#6778 = EDGE_CURVE ( 'NONE', #10266, #1842, #4127, .T. ) ;
#6779 = ORIENTED_EDGE ( 'NONE', *, *, #9163, .T. ) ;
#6780 = ADVANCED_FACE ( 'NONE', ( #4072 ), #7007, .T. ) ;
#6781 = EDGE_CURVE ( 'NONE', #7263, #4273, #10171, .T. ) ;
#6782 = EDGE_CURVE ( 'NONE', #7160, #7364, #4942, .T. ) ;
#6783 = AXIS2_PLACEMENT_3D ( 'NONE', #1470, #5282, #9107 ) ;
#6784 = CARTESIAN_POINT ( 'NONE',  ( 0.000000000000000000, 4.576198416197252428, 26.60936692326691499 ) ) ;
#6785 = DIRECTION ( 'NONE',  ( -1.000000000000000000, 0.000000000000000000, 0.000000000000000000 ) ) ;
#6786 = AXIS2_PLACEMENT_3D ( 'NONE', #2110, #3397, #7807 ) ;
#6787 = CIRCLE ( 'NONE', #987, 0.7499999999999997780 ) ;
#6788 = DIRECTION ( 'NONE',  ( -1.000000000000000000, -0.000000000000000000, -0.000000000000000000 ) ) ;
#6789 = CARTESIAN_POINT ( 'NONE',  ( -36.00000000000000711, 0.000000000000000000, 0.000000000000000000 ) ) ;
#6790 = ORIENTED_EDGE ( 'NONE', *, *, #3933, .F. ) ;
#6791 = ORIENTED_EDGE ( 'NONE', *, *, #11883, .T. ) ;
#6792 = ORIENTED_EDGE ( 'NONE', *, *, #8994, .F. ) ;
#6793 = DIRECTION ( 'NONE',  ( 1.000000000000000000, 0.000000000000000000, 0.000000000000000000 ) ) ;
#6794 = EDGE_CURVE ( 'NONE', #7247, #11219, #9582, .T. ) ;
#6795 = ORIENTED_EDGE ( 'NONE', *, *, #5408, .T. ) ;
#6796 = AXIS2_PLACEMENT_3D ( 'NONE', #11267, #6584, #2900 ) ;
#6797 = VECTOR ( 'NONE', #8315, 1000.000000000000000 ) ;
#6798 = CIRCLE ( 'NONE', #7394, 0.1000000000000002554 ) ;
#6799 = ORIENTED_EDGE ( 'NONE', *, *, #4699, .F. ) ;
#6800 = ORIENTED_EDGE ( 'NONE', *, *, #4244, .T. ) ;
#6801 = CARTESIAN_POINT ( 'NONE',  ( -3.309651814758565180, -5.455921364805393026, -1.000000000000000000 ) ) ;
#6802 = DIRECTION ( 'NONE',  ( 0.000000000000000000, -0.000000000000000000, 1.000000000000000000 ) ) ;
#6803 = CARTESIAN_POINT ( 'NONE',  ( 0.000000000000000000, 0.000000000000000000, 0.000000000000000000 ) ) ;
#6804 = CARTESIAN_POINT ( 'NONE',  ( 37.00000000000000711, 1.456773409934505593E-31, -36.99999999999998579 ) ) ;
#6805 = CIRCLE ( 'NONE', #5584, 21.00000000002100009 ) ;
#6806 = ORIENTED_EDGE ( 'NONE', *, *, #2320, .F. ) ;
#6807 = AXIS2_PLACEMENT_3D ( 'NONE', #1878, #11614, #1065 ) ;
#6808 = DIRECTION ( 'NONE',  ( -1.734723475976807094E-16, 1.000000000000000000, 0.000000000000000000 ) ) ;
#6809 = EDGE_LOOP ( 'NONE', ( #9106, #1223, #6929, #6182 ) ) ;
#6810 = SHAPE_REPRESENTATION_RELATIONSHIP ( 'NONE' , 'NONE' ,  #5877, #7504 ) ;
#6811 = EDGE_CURVE ( 'NONE', #8658, #7148, #2386, .T. ) ;
#6813 = EDGE_CURVE ( 'NONE', #5310, #978, #10572, .T. ) ;
#6812 = ORIENTED_EDGE ( 'NONE', *, *, #4195, .F. ) ;
#6814 = CARTESIAN_POINT ( 'NONE',  ( 4.999999999999999112, 8.872489362018390224, -14.40062958310456054 ) ) ;
#6815 = ORIENTED_EDGE ( 'NONE', *, *, #9151, .F. ) ;
#6816 = DIRECTION ( 'NONE',  ( 0.000000000000000000, 0.000000000000000000, 1.000000000000000000 ) ) ;
#6817 = AXIS2_PLACEMENT_3D ( 'NONE', #1848, #3031, #8785 ) ;
#6818 = CIRCLE ( 'NONE', #10002, 6.750000000000000000 ) ;
#6819 = AXIS2_PLACEMENT_3D ( 'NONE', #2339, #10048, #10856 ) ;
#6820 = DIRECTION ( 'NONE',  ( -1.000000000000000000, 0.000000000000000000, -0.000000000000000000 ) ) ;
#6821 = EDGE_LOOP ( 'NONE', ( #5052, #465 ) ) ;
#6822 = CARTESIAN_POINT ( 'NONE',  ( 42.00000000000000000, -2.824006678639516377, 3.881363971466655904 ) ) ;
#6823 = CARTESIAN_POINT ( 'NONE',  ( 4.999999999999999112, -6.283573709965446064, 19.24938187143294144 ) ) ;
#6824 = AXIS2_PLACEMENT_3D ( 'NONE', #3143, #2309, #10754 ) ;
#6825 = EDGE_LOOP ( 'NONE', ( #9948, #8119 ) ) ;
#6826 = AXIS2_PLACEMENT_3D ( 'NONE', #3836, #9719, #5762 ) ;
#6827 = CARTESIAN_POINT ( 'NONE',  ( 45.00000000000000000, 0.000000000000000000, 0.000000000000000000 ) ) ;
#6828 = APPLICATION_PROTOCOL_DEFINITION ( 'draft international standard', 'automotive_design', 1998, #10723 ) ;
#6829 = DIRECTION ( 'NONE',  ( 0.000000000000000000, 0.000000000000000000, 1.000000000000000000 ) ) ;
#6830 = AXIS2_PLACEMENT_3D ( 'NONE', #3406, #584, #11150 ) ;
#6831 = CIRCLE ( 'NONE', #5438, 7.000000000000006217 ) ;
#6832 = DIRECTION ( 'NONE',  ( -1.000000000000000000, 0.000000000000000000, 0.000000000000000000 ) ) ;
#6833 = EDGE_LOOP ( 'NONE', ( #4111, #1267 ) ) ;
#6834 = CIRCLE ( 'NONE', #11606, 14.24900000001425404 ) ;
#6835 = AXIS2_PLACEMENT_3D ( 'NONE', #11998, #4508, #2747 ) ;
#6836 = PRODUCT ( 'spur gear_iso_ISO - Spur gear 3M 12T 20PA 5FW ---S12A75H50L10.0S1', 'spur gear_iso_ISO - Spur gear 3M 12T 20PA 5FW ---S12A75H50L10.0S1', '', ( #5538 ) ) ;
#6837 = AXIS2_PLACEMENT_3D ( 'NONE', #1914, #10588, #9597 ) ;
#6838 = CIRCLE ( 'NONE', #5225, 7.000000000000006217 ) ;
#6839 = FACE_OUTER_BOUND ( 'NONE', #2976, .T. ) ;
#6840 = LINE ( 'NONE', #3200, #1407 ) ;
#6841 = ADVANCED_FACE ( 'NONE', ( #10992 ), #10125, .T. ) ;
#6842 = DIRECTION ( 'NONE',  ( 0.000000000000000000, 1.000000000000000000, 0.000000000000000000 ) ) ;
#6843 = DIRECTION ( 'NONE',  ( 0.000000000000000000, -1.000000000000000000, 0.000000000000000000 ) ) ;
#6844 = ORIENTED_EDGE ( 'NONE', *, *, #60, .T. ) ;
#6845 = EDGE_CURVE ( 'NONE', #10053, #8252, #580, .T. ) ;
#6846 = CARTESIAN_POINT ( 'NONE',  ( 42.00000000000000000, 7.000000000000004441, -41.99999999999998579 ) ) ;
#6847 = DIRECTION ( 'NONE',  ( -1.000000000000000000, 0.000000000000000000, 0.000000000000000000 ) ) ;
#6848 = CIRCLE ( 'NONE', #7847, 5.000000000000000000 ) ;
#6849 = VERTEX_POINT ( 'NONE', #7443 ) ;
#6850 = CYLINDRICAL_SURFACE ( 'NONE', #4882, 5.000000000000000000 ) ;
#6851 = AXIS2_PLACEMENT_3D ( 'NONE', #2181, #5177, #7001 ) ;
#6852 = VECTOR ( 'NONE', #1082, 1000.000000000000000 ) ;
#6853 = ORIENTED_EDGE ( 'NONE', *, *, #10054, .F. ) ;
#6854 = DIRECTION ( 'NONE',  ( 1.000000000000000000, -0.000000000000000000, -0.000000000000000000 ) ) ;
#6855 = AXIS2_PLACEMENT_3D ( 'NONE', #11521, #10666, #9791 ) ;
#6856 = DIRECTION ( 'NONE',  ( 0.000000000000000000, 0.000000000000000000, 1.000000000000000000 ) ) ;
#6857 = LINE ( 'NONE', #3218, #762 ) ;
#6858 = EDGE_CURVE ( 'NONE', #661, #3785, #3788, .T. ) ;
#6859 = CIRCLE ( 'NONE', #454, 2.149999999999999023 ) ;
#6860 = LINE ( 'NONE', #2093, #1441 ) ;
#6861 = DIRECTION ( 'NONE',  ( -0.000000000000000000, 1.000000000000000000, -0.000000000000000000 ) ) ;
#6862 = VERTEX_POINT ( 'NONE', #10004 ) ;
#6863 = ADVANCED_FACE ( 'NONE', ( #2431 ), #2544, .T. ) ;
#6864 = EDGE_CURVE ( 'NONE', #5720, #7438, #12156, .T. ) ;
#6865 = EDGE_LOOP ( 'NONE', ( #7868, #455, #156, #9120 ) ) ;
#6866 = EDGE_LOOP ( 'NONE', ( #5380, #6217, #512, #6202 ) ) ;
#6867 = CIRCLE ( 'NONE', #4449, 20.24900000002024569 ) ;
#6868 = AXIS2_PLACEMENT_3D ( 'NONE', #3511, #2504, #555 ) ;
#6869 = LINE ( 'NONE', #9972, #11162 ) ;
#6870 = ORIENTED_EDGE ( 'NONE', *, *, #12044, .F. ) ;
#6871 = DIRECTION ( 'NONE',  ( 0.000000000000000000, 0.000000000000000000, -1.000000000000000000 ) ) ;
#6872 = CARTESIAN_POINT ( 'NONE',  ( 0.000000000000000000, -14.41081992069293349, -22.83261415639518432 ) ) ;
#6873 = CARTESIAN_POINT ( 'NONE',  ( 0.000000000000000000, 3.306546357697853733E-16, -2.700000000000000178 ) ) ;
#6874 = DIRECTION ( 'NONE',  ( -1.000000000000000000, 0.000000000000000000, 0.000000000000000000 ) ) ;
#6875 = VERTEX_POINT ( 'NONE', #4553 ) ;
#6876 = COLOUR_RGB ( '',1.000000000000000000, 0.9490196078431372140, 0.9098039215686274384 ) ;
#6877 = DIRECTION ( 'NONE',  ( 1.000000000000000000, -0.000000000000000000, -0.000000000000000000 ) ) ;
#6878 = PRODUCT_DEFINITION ( 'UNKNOWN', '', #10840, #10656 ) ;
#6879 = ORIENTED_EDGE ( 'NONE', *, *, #8240, .F. ) ;
#6880 =( LENGTH_UNIT ( ) NAMED_UNIT ( * ) SI_UNIT ( .MILLI., .METRE. ) );
#6881 = ORIENTED_EDGE ( 'NONE', *, *, #10154, .T. ) ;
#6882 = CYLINDRICAL_SURFACE ( 'NONE', #11597, 14.24900000001425227 ) ;
#6883 = ORIENTED_EDGE ( 'NONE', *, *, #6313, .T. ) ;
#6884 = DIRECTION ( 'NONE',  ( 1.000000000000000000, -0.000000000000000000, -0.000000000000000000 ) ) ;
#6885 = CYLINDRICAL_SURFACE ( 'NONE', #2011, 4.800000000000000711 ) ;
#6886 = EDGE_CURVE ( 'NONE', #4099, #3713, #5441, .T. ) ;
#6887 = EDGE_CURVE ( 'NONE', #7155, #4621, #1387, .T. ) ;
#6888 = ORIENTED_EDGE ( 'NONE', *, *, #11947, .T. ) ;
#6889 = DIRECTION ( 'NONE',  ( 0.000000000000000000, 0.000000000000000000, -1.000000000000000000 ) ) ;
#6890 = LINE ( 'NONE', #8942, #2654 ) ;
#6891 = VERTEX_POINT ( 'NONE', #10073 ) ;
#6892 =( NAMED_UNIT ( * ) SI_UNIT ( $, .STERADIAN. ) SOLID_ANGLE_UNIT ( ) );
#6893 = CIRCLE ( 'NONE', #7485, 7.200000000007200640 ) ;
#6894 = SURFACE_STYLE_FILL_AREA ( #3080 ) ;
#6895 = DIRECTION ( 'NONE',  ( -1.000000000000000000, -0.000000000000000000, -0.000000000000000000 ) ) ;
#6896 = CYLINDRICAL_SURFACE ( 'NONE', #5690, 40.00000000000000711 ) ;
#6897 = ORIENTED_EDGE ( 'NONE', *, *, #4580, .F. ) ;
#6898 = DIRECTION ( 'NONE',  ( -1.000000000000000000, 0.000000000000000000, 0.000000000000000000 ) ) ;
#6899 = AXIS2_PLACEMENT_3D ( 'NONE', #6457, #9276, #10940 ) ;
#6900 =( LENGTH_UNIT ( ) NAMED_UNIT ( * ) SI_UNIT ( .MILLI., .METRE. ) );
#6901 = DIRECTION ( 'NONE',  ( -1.000000000000000000, -0.000000000000000000, -0.000000000000000000 ) ) ;
#6902 = FACE_OUTER_BOUND ( 'NONE', #5340, .T. ) ;
#6903 = CARTESIAN_POINT ( 'NONE',  ( 51.00000000000000000, 3.500000000000001332, -38.49999999999998579 ) ) ;
#6904 = VERTEX_POINT ( 'NONE', #8264 ) ;
#6905 = DIRECTION ( 'NONE',  ( -1.000000000000000000, -0.000000000000000000, -0.000000000000000000 ) ) ;
#6906 = DIRECTION ( 'NONE',  ( 0.000000000000000000, 0.000000000000000000, 1.000000000000000000 ) ) ;
#6907 = EDGE_LOOP ( 'NONE', ( #12035, #11104, #11879, #8869 ) ) ;
#6908 = DIRECTION ( 'NONE',  ( 0.000000000000000000, 0.3826834323650841752, 0.9238795325112890700 ) ) ;
#6909 = VECTOR ( 'NONE', #792, 1000.000000000000000 ) ;
#6910 = ORIENTED_EDGE ( 'NONE', *, *, #414, .T. ) ;
#6911 = CARTESIAN_POINT ( 'NONE',  ( -1.499999999999999556, 6.975000000000000533, 0.000000000000000000 ) ) ;
#6912 = CARTESIAN_POINT ( 'NONE',  ( 1.250000000000000000, -6.429618962271402616, -1.000000000000000000 ) ) ;
#6913 = LINE ( 'NONE', #2324, #10746 ) ;
#6914 = DIRECTION ( 'NONE',  ( 0.000000000000000000, 0.000000000000000000, -1.000000000000000000 ) ) ;
#6915 = CARTESIAN_POINT ( 'NONE',  ( 70.79898987322334847, -3.499999999999998668, -38.49999999999998579 ) ) ;
#6916 = ORIENTED_EDGE ( 'NONE', *, *, #12265, .F. ) ;
#6917 = FILL_AREA_STYLE_COLOUR ( '', #3859 ) ;
#6918 = ORIENTED_EDGE ( 'NONE', *, *, #11050, .T. ) ;
#6919 = APPLICATION_PROTOCOL_DEFINITION ( 'draft international standard', 'automotive_design', 1998, #2570 ) ;
#6920 = ORIENTED_EDGE ( 'NONE', *, *, #8854, .F. ) ;
#6921 = EDGE_CURVE ( 'NONE', #3765, #8559, #9783, .T. ) ;
#6922 = EDGE_CURVE ( 'NONE', #9598, #6404, #11172, .T. ) ;
#6923 = DIRECTION ( 'NONE',  ( 0.000000000000000000, -1.224646799147353454E-16, 1.000000000000000000 ) ) ;
#6924 = ORIENTED_EDGE ( 'NONE', *, *, #12157, .F. ) ;
#6925 = DIRECTION ( 'NONE',  ( 0.000000000000000000, 0.000000000000000000, 1.000000000000000000 ) ) ;
#6926 = CARTESIAN_POINT ( 'NONE',  ( 0.4798950312200447876, 0.5999999999999998668, -3.611246565534919739 ) ) ;
#6927 = DIRECTION ( 'NONE',  ( -1.000000000000000000, -0.000000000000000000, -0.000000000000000000 ) ) ;
#6928 = DIRECTION ( 'NONE',  ( 1.000000000000000000, 0.000000000000000000, 0.000000000000000000 ) ) ;
#6929 = ORIENTED_EDGE ( 'NONE', *, *, #8614, .T. ) ;
#6930 = VERTEX_POINT ( 'NONE', #5313 ) ;
#6931 = ORIENTED_EDGE ( 'NONE', *, *, #6981, .F. ) ;
#6932 = CYLINDRICAL_SURFACE ( 'NONE', #7031, 7.200000000007202416 ) ;
#6933 = EDGE_CURVE ( 'NONE', #5247, #9896, #10772, .T. ) ;
#6934 = ORIENTED_EDGE ( 'NONE', *, *, #485, .T. ) ;
#6935 = DIRECTION ( 'NONE',  ( 0.000000000000000000, 0.000000000000000000, -1.000000000000000000 ) ) ;
#6936 = ADVANCED_FACE ( 'NONE', ( #6367 ), #9321, .T. ) ;
#6937 = EDGE_CURVE ( 'NONE', #9068, #5793, #5985, .T. ) ;
#6938 = ADVANCED_FACE ( 'NONE', ( #7266 ), #5256, .T. ) ;
#6939 = CARTESIAN_POINT ( 'NONE',  ( 45.00000000000001421, 46.00000000000001421, -46.00000000000000000 ) ) ;
#6940 = ORIENTED_EDGE ( 'NONE', *, *, #11655, .T. ) ;
#6941 = DIRECTION ( 'NONE',  ( 1.000000000000000000, 0.000000000000000000, 0.000000000000000000 ) ) ;
#6942 = LINE ( 'NONE', #7755, #9266 ) ;
#6943 = ORIENTED_EDGE ( 'NONE', *, *, #1496, .F. ) ;
#6944 = DIRECTION ( 'NONE',  ( -1.000000000000000000, 0.000000000000000000, 0.000000000000000000 ) ) ;
#6945 = DIRECTION ( 'NONE',  ( 1.000000000000000000, 0.000000000000000000, 0.000000000000000000 ) ) ;
#6946 = CARTESIAN_POINT ( 'NONE',  ( 1.000000000000000000, -0.6000000000000001998, 3.826895796574397046 ) ) ;
#6947 = EDGE_CURVE ( 'NONE', #9895, #3834, #4556, .T. ) ;
#6948 = ORIENTED_EDGE ( 'NONE', *, *, #8631, .T. ) ;
#6949 = DIRECTION ( 'NONE',  ( 1.000000000000000000, -0.000000000000000000, -0.000000000000000000 ) ) ;
#6950 = LINE ( 'NONE', #3268, #5414 ) ;
#6951 = DIRECTION ( 'NONE',  ( 1.000000000000000000, 0.000000000000000000, 0.000000000000000000 ) ) ;
#6952 = CARTESIAN_POINT ( 'NONE',  ( 4.999999999999999112, 20.18872947935930995, -1.561154383803291967 ) ) ;
#6953 = CARTESIAN_POINT ( 'NONE',  ( 4.999999999999999112, 4.916402349214867407, -20.41639017900854469 ) ) ;
#6954 = ORIENTED_EDGE ( 'NONE', *, *, #5930, .T. ) ;
#6955 = DIRECTION ( 'NONE',  ( -1.000000000000000000, -0.000000000000000000, -0.000000000000000000 ) ) ;
#6956 = CARTESIAN_POINT ( 'NONE',  ( 43.00000000000000000, 3.792354139917828437, 2.942456469932579921 ) ) ;
#6957 = ORIENTED_EDGE ( 'NONE', *, *, #463, .F. ) ;
#6958 = FACE_OUTER_BOUND ( 'NONE', #6821, .T. ) ;
#6959 = EDGE_CURVE ( 'NONE', #5098, #477, #10155, .T. ) ;
#6960 = ORIENTED_EDGE ( 'NONE', *, *, #6717, .F. ) ;
#6961 = DIRECTION ( 'NONE',  ( -1.000000000000000000, 0.000000000000000000, 0.000000000000000000 ) ) ;
#6962 = VECTOR ( 'NONE', #10713, 999.9999999999998863 ) ;
#6963 = SURFACE_SIDE_STYLE ('',( #9958 ) ) ;
#6964 = DIRECTION ( 'NONE',  ( 1.000000000000000000, 0.000000000000000000, 0.000000000000000000 ) ) ;
#6965 = CARTESIAN_POINT ( 'NONE',  ( 1.500000000000000444, 5.100000000000000533, 0.000000000000000000 ) ) ;
#6966 = FACE_OUTER_BOUND ( 'NONE', #7939, .T. ) ;
#6967 = CIRCLE ( 'NONE', #167, 5.525000000000000355 ) ;
#6968 = CIRCLE ( 'NONE', #1569, 14.24900000001425227 ) ;
#6969 = ORIENTED_EDGE ( 'NONE', *, *, #5307, .T. ) ;
#6970 = VERTEX_POINT ( 'NONE', #7506 ) ;
#6971 = FACE_BOUND ( 'NONE', #6833, .T. ) ;
#6972 = EDGE_LOOP ( 'NONE', ( #1989, #48, #3474, #11312 ) ) ;
#6973 = VECTOR ( 'NONE', #2644, 1000.000000000000000 ) ;
#6974 = AXIS2_PLACEMENT_3D ( 'NONE', #4736, #2056, #6747 ) ;
#6975 = ORIENTED_EDGE ( 'NONE', *, *, #2910, .F. ) ;
#6976 = ORIENTED_EDGE ( 'NONE', *, *, #807, .F. ) ;
#6977 = CARTESIAN_POINT ( 'NONE',  ( 36.00000000000000711, -2.534184013771451305, 4.310210132272582761 ) ) ;
#6978 = DIRECTION ( 'NONE',  ( 1.000000000000000000, 0.000000000000000000, 0.000000000000000000 ) ) ;
#6979 = LINE ( 'NONE', #7875, #7627 ) ;
#6980 = CYLINDRICAL_SURFACE ( 'NONE', #10607, 7.200000000007202416 ) ;
#6981 = EDGE_CURVE ( 'NONE', #8609, #4760, #9444, .T. ) ;
#6982 = VERTEX_POINT ( 'NONE', #2877 ) ;
#6983 = CIRCLE ( 'NONE', #1997, 5.000000000000000000 ) ;
#6984 = ORIENTED_EDGE ( 'NONE', *, *, #3947, .T. ) ;
#6985 = VECTOR ( 'NONE', #7831, 1000.000000000000000 ) ;
#6986 = EDGE_CURVE ( 'NONE', #3187, #4264, #563, .T. ) ;
#6987 = ORIENTED_EDGE ( 'NONE', *, *, #4930, .F. ) ;
#6988 = CIRCLE ( 'NONE', #190, 27.00000000002699707 ) ;
#6989 = CARTESIAN_POINT ( 'NONE',  ( 14.40000000000000036, 2.000000000000000000, 0.000000000000000000 ) ) ;
#6990 = CARTESIAN_POINT ( 'NONE',  ( 0.000000000000000000, 0.000000000000000000, 0.000000000000000000 ) ) ;
#6991 = AXIS2_PLACEMENT_3D ( 'NONE', #4152, #7979, #7925 ) ;
#6992 = CARTESIAN_POINT ( 'NONE',  ( 3.678949249685231848, 0.000000000000000000, 0.000000000000000000 ) ) ;
#6993 = CIRCLE ( 'NONE', #8992, 0.7499999999999997780 ) ;
#6994 = ADVANCED_FACE ( 'NONE', ( #867 ), #6505, .T. ) ;
#6995 = ORIENTED_EDGE ( 'NONE', *, *, #148, .F. ) ;
#6996 = FACE_OUTER_BOUND ( 'NONE', #9538, .T. ) ;
#6997 = DIRECTION ( 'NONE',  ( -1.000000000000000000, -0.000000000000000000, 0.000000000000000000 ) ) ;
#6998 = VERTEX_POINT ( 'NONE', #5553 ) ;
#6999 = CARTESIAN_POINT ( 'NONE',  ( 0.000000000000000000, -26.33508479058324880, 5.955107813822411167 ) ) ;
#7000 = EDGE_CURVE ( 'NONE', #2800, #4492, #6556, .T. ) ;
#7001 = DIRECTION ( 'NONE',  ( 0.000000000000000000, 0.000000000000000000, 1.000000000000000000 ) ) ;
#7002 = EDGE_CURVE ( 'NONE', #2114, #1494, #9765, .T. ) ;
#7003 = AXIS2_PLACEMENT_3D ( 'NONE', #5393, #11260, #7214 ) ;
#7004 = CARTESIAN_POINT ( 'NONE',  ( 0.000000000000000000, 0.000000000000000000, 0.000000000000000000 ) ) ;
#7005 = AXIS2_PLACEMENT_3D ( 'NONE', #9945, #6078, #2132 ) ;
#7006 = ORIENTED_EDGE ( 'NONE', *, *, #8852, .F. ) ;
#7007 = CYLINDRICAL_SURFACE ( 'NONE', #8787, 40.00000000000000711 ) ;
#7008 = AXIS2_PLACEMENT_3D ( 'NONE', #11117, #11246, #6371 ) ;
#7009 = EDGE_CURVE ( 'NONE', #5192, #7138, #10344, .T. ) ;
#7010 = DIRECTION ( 'NONE',  ( 0.000000000000000000, 0.000000000000000000, -1.000000000000000000 ) ) ;
#7011 = AXIS2_PLACEMENT_3D ( 'NONE', #2894, #9713, #7578 ) ;
#7012 = DIRECTION ( 'NONE',  ( 1.000000000000000000, 0.000000000000000000, 0.000000000000000000 ) ) ;
#7013 = FACE_OUTER_BOUND ( 'NONE', #9320, .T. ) ;
#7014 = AXIS2_PLACEMENT_3D ( 'NONE', #8927, #7982, #6233 ) ;
#7015 = VECTOR ( 'NONE', #11474, 1000.000000000000000 ) ;
#7016 = CARTESIAN_POINT ( 'NONE',  ( 0.5000000000000000000, -6.429618962271402616, -1.000000000000000000 ) ) ;
#7017 = CARTESIAN_POINT ( 'NONE',  ( -26.00000000000000355, 0.000000000000000000, 40.00000000000000711 ) ) ;
#7018 = ORIENTED_EDGE ( 'NONE', *, *, #8398, .T. ) ;
#7019 = VERTEX_POINT ( 'NONE', #10494 ) ;
#7020 = CARTESIAN_POINT ( 'NONE',  ( 0.000000000000000000, 26.60936692326690789, 4.576198416197345686 ) ) ;
#7021 = DIRECTION ( 'NONE',  ( -1.000000000000000000, -0.000000000000000000, 0.000000000000000000 ) ) ;
#7022 = ORIENTED_EDGE ( 'NONE', *, *, #7887, .T. ) ;
#7023 = DIRECTION ( 'NONE',  ( 0.000000000000000000, 0.000000000000000000, 1.000000000000000000 ) ) ;
#7024 = PRODUCT_DEFINITION_CONTEXT ( 'detailed design', #672, 'design' ) ;
#7025 = EDGE_LOOP ( 'NONE', ( #10650, #12020, #4204, #180 ) ) ;
#7026 = DIRECTION ( 'NONE',  ( -1.000000000000000000, -0.000000000000000000, -0.000000000000000000 ) ) ;
#7027 =( GEOMETRIC_REPRESENTATION_CONTEXT ( 3 ) GLOBAL_UNCERTAINTY_ASSIGNED_CONTEXT ( ( #5766 ) ) GLOBAL_UNIT_ASSIGNED_CONTEXT ( ( #3888, #4750, #2746 ) ) REPRESENTATION_CONTEXT ( 'NONE', 'WORKASPACE' ) );
#7028 = AXIS2_PLACEMENT_3D ( 'NONE', #4733, #8553, #7620 ) ;
#7029 = AXIS2_PLACEMENT_3D ( 'NONE', #4763, #140, #3901 ) ;
#7030 = AXIS2_PLACEMENT_3D ( 'NONE', #4143, #8915, #2146 ) ;
#7031 = AXIS2_PLACEMENT_3D ( 'NONE', #10734, #2060, #1236 ) ;
#7032 = DIRECTION ( 'NONE',  ( 0.000000000000000000, 0.000000000000000000, 1.000000000000000000 ) ) ;
#7033 = DIRECTION ( 'NONE',  ( -1.000000000000000000, -0.000000000000000000, -0.000000000000000000 ) ) ;
#7034 = EDGE_CURVE ( 'NONE', #4033, #9147, #5966, .T. ) ;
#7035 = ADVANCED_FACE ( 'NONE', ( #3931 ), #9632, .F. ) ;
#7036 = DIRECTION ( 'NONE',  ( 0.000000000000000000, 0.000000000000000000, -1.000000000000000000 ) ) ;
#7037 = CARTESIAN_POINT ( 'NONE',  ( 0.000000000000000000, -14.88411597386723351, -8.035066368449358620 ) ) ;
#7038 = VECTOR ( 'NONE', #716, 1000.000000000000000 ) ;
#7039 = PRODUCT_DEFINITION_SHAPE ( 'NONE', 'NONE',  #12357 ) ;
#7040 = EDGE_LOOP ( 'NONE', ( #10191, #9049, #6897, #6329 ) ) ;
#7041 = VECTOR ( 'NONE', #6719, 1000.000000000000000 ) ;
#7042 = VERTEX_POINT ( 'NONE', #11358 ) ;
#7043 = CYLINDRICAL_SURFACE ( 'NONE', #683, 5.000000000000004441 ) ;
#7044 = VERTEX_POINT ( 'NONE', #5686 ) ;
#7045 = STYLED_ITEM ( 'NONE', ( #3418 ), #6462 ) ;
#7046 = AXIS2_PLACEMENT_3D ( 'NONE', #6965, #4142, #7036 ) ;
#7047 = AXIS2_PLACEMENT_3D ( 'NONE', #3315, #3137, #7071 ) ;
#7048 = CIRCLE ( 'NONE', #10845, 7.200000000007202416 ) ;
#7049 = EDGE_LOOP ( 'NONE', ( #9995, #3564, #7189, #4667 ) ) ;
#7050 = CARTESIAN_POINT ( 'NONE',  ( 0.000000000000000000, 0.000000000000000000, 0.000000000000000000 ) ) ;
#7051 = DIRECTION ( 'NONE',  ( 0.000000000000000000, 0.000000000000000000, 1.000000000000000000 ) ) ;
#7052 = CARTESIAN_POINT ( 'NONE',  ( 50.00005079999999680, 0.000000000000000000, 5.000000000000000000 ) ) ;
#7053 = CARTESIAN_POINT ( 'NONE',  ( 4.999999999999999112, -13.17168466712939257, 15.37949036966207039 ) ) ;
#7054 = ORIENTED_EDGE ( 'NONE', *, *, #1272, .T. ) ;
#7055 = DIRECTION ( 'NONE',  ( -0.000000000000000000, 1.000000000000000000, -0.000000000000000000 ) ) ;
#7056 = CIRCLE ( 'NONE', #9063, 12.50000000000000000 ) ;
#7057 = ORIENTED_EDGE ( 'NONE', *, *, #9919, .T. ) ;
#7058 = VECTOR ( 'NONE', #8512, 1000.000000000000000 ) ;
#7059 = ORIENTED_EDGE ( 'NONE', *, *, #1742, .F. ) ;
#7060 = DIRECTION ( 'NONE',  ( -1.000000000000000000, 0.000000000000000000, 0.000000000000000000 ) ) ;
#7061 = DIRECTION ( 'NONE',  ( 0.000000000000000000, 0.5000000000000012212, 0.8660254037844380415 ) ) ;
#7062 = ADVANCED_BREP_SHAPE_REPRESENTATION ( '', ( #349, #6056 ), #2232 ) ;
#7063 = DIRECTION ( 'NONE',  ( -4.000869187770762975E-18, -0.8386705679454229401, -0.5446390350150287496 ) ) ;
#7064 = EDGE_CURVE ( 'NONE', #3765, #611, #9956, .T. ) ;
#7065 = PRESENTATION_LAYER_ASSIGNMENT (  '', '', ( #3083 ) ) ;
#7066 = ORIENTED_EDGE ( 'NONE', *, *, #366, .T. ) ;
#7067 = CARTESIAN_POINT ( 'NONE',  ( 4.999999999999999112, 22.05152472667129970, 15.57980286237480350 ) ) ;
#7068 = ORIENTED_EDGE ( 'NONE', *, *, #9209, .F. ) ;
#7069 = FILL_AREA_STYLE ('',( #6421 ) ) ;
#7070 =( NAMED_UNIT ( * ) PLANE_ANGLE_UNIT ( ) SI_UNIT ( $, .RADIAN. ) );
#7071 = DIRECTION ( 'NONE',  ( 0.000000000000000000, 0.9238795325112850731, 0.3826834323650936676 ) ) ;
#7072 = CARTESIAN_POINT ( 'NONE',  ( -1.500000000000001332, 0.000000000000000000, 0.000000000000000000 ) ) ;
#7073 = VECTOR ( 'NONE', #4176, 1000.000000000000000 ) ;
#7074 = ORIENTED_EDGE ( 'NONE', *, *, #4773, .F. ) ;
#7075 = DIRECTION ( 'NONE',  ( -1.000000000000000000, -0.000000000000000000, 0.000000000000000000 ) ) ;
#7076 = ADVANCED_FACE ( 'NONE', ( #9375 ), #2683, .T. ) ;
#7077 = DIRECTION ( 'NONE',  ( 1.000000000000000000, 0.000000000000000000, -0.000000000000000000 ) ) ;
#7078 = ADVANCED_FACE ( 'NONE', ( #990 ), #7564, .T. ) ;
#7079 = EDGE_CURVE ( 'NONE', #8658, #2298, #10433, .T. ) ;
#7080 =( NAMED_UNIT ( * ) SI_UNIT ( $, .STERADIAN. ) SOLID_ANGLE_UNIT ( ) );
#7081 = CARTESIAN_POINT ( 'NONE',  ( 4.999999999999999112, -13.17168466712917585, -15.37949036966225513 ) ) ;
#7082 = AXIS2_PLACEMENT_3D ( 'NONE', #6602, #4723, #964 ) ;
#7083 = FACE_OUTER_BOUND ( 'NONE', #8816, .T. ) ;
#7084 = DIRECTION ( 'NONE',  ( 1.000000000000000000, 0.000000000000000000, 0.000000000000000000 ) ) ;
#7085 = ORIENTED_EDGE ( 'NONE', *, *, #4761, .T. ) ;
#7086 = ORIENTED_EDGE ( 'NONE', *, *, #4088, .F. ) ;
#7087 = DIRECTION ( 'NONE',  ( 0.000000000000000000, -0.8660254037844328234, -0.5000000000000101030 ) ) ;
#7088 = DIRECTION ( 'NONE',  ( 0.000000000000000000, -1.000000000000000000, 0.000000000000000000 ) ) ;
#7089 = ORIENTED_EDGE ( 'NONE', *, *, #965, .F. ) ;
#7090 = FACE_BOUND ( 'NONE', #8517, .T. ) ;
#7091 = ORIENTED_EDGE ( 'NONE', *, *, #11134, .T. ) ;
#7092 = DIRECTION ( 'NONE',  ( 0.000000000000000000, 0.000000000000000000, 1.000000000000000000 ) ) ;
#7093 = CIRCLE ( 'NONE', #12057, 20.24900000002024569 ) ;
#7094 = ADVANCED_FACE ( 'NONE', ( #794 ), #4622, .F. ) ;
#7095 = EDGE_CURVE ( 'NONE', #611, #2076, #929, .T. ) ;
#7096 = EDGE_CURVE ( 'NONE', #10859, #1263, #5556, .T. ) ;
#7097 = CARTESIAN_POINT ( 'NONE',  ( -10.00000000000000000, 0.000000000000000000, 0.000000000000000000 ) ) ;
#7098 = FACE_BOUND ( 'NONE', #373, .T. ) ;
#7099 = DIRECTION ( 'NONE',  ( 0.000000000000000000, 0.7071067811865486830, -0.7071067811865464625 ) ) ;
#7100 = ORIENTED_EDGE ( 'NONE', *, *, #12154, .F. ) ;
#7101 = CIRCLE ( 'NONE', #6502, 20.24900000002024569 ) ;
#7102 = CARTESIAN_POINT ( 'NONE',  ( 4.999999999999999112, 4.576198416197251539, 26.60936692326691855 ) ) ;
#7103 = ORIENTED_EDGE ( 'NONE', *, *, #4320, .T. ) ;
#7104 = DIRECTION ( 'NONE',  ( 0.000000000000000000, 0.000000000000000000, -1.000000000000000000 ) ) ;
#7105 = ORIENTED_EDGE ( 'NONE', *, *, #6372, .F. ) ;
#7106 = EDGE_CURVE ( 'NONE', #12088, #10665, #11339, .T. ) ;
#7107 = EDGE_CURVE ( 'NONE', #1798, #1083, #11537, .T. ) ;
#7108 = ORIENTED_EDGE ( 'NONE', *, *, #547, .F. ) ;
#7109 = CIRCLE ( 'NONE', #1912, 7.200000000007202416 ) ;
#7110 = DIRECTION ( 'NONE',  ( 0.000000000000000000, -0.3826834323650971648, 0.9238795325112837409 ) ) ;
#7111 = CARTESIAN_POINT ( 'NONE',  ( 37.00000000000000711, 3.183245106666227286, -38.14423151746819229 ) ) ;
#7112 = DIRECTION ( 'NONE',  ( 1.000000000000000000, -0.000000000000000000, -0.000000000000000000 ) ) ;
#7113 = DIRECTION ( 'NONE',  ( 1.000000000000000000, 0.000000000000000000, 0.000000000000000000 ) ) ;
#7114 = ORIENTED_EDGE ( 'NONE', *, *, #9531, .F. ) ;
#7115 = CARTESIAN_POINT ( 'NONE',  ( -15.00000000000000000, 30.00000000000000711, 0.000000000000000000 ) ) ;
#7116 = ORIENTED_EDGE ( 'NONE', *, *, #10580, .F. ) ;
#7117 = CARTESIAN_POINT ( 'NONE',  ( 37.00000000000000711, 0.000000000000000000, 0.000000000000000000 ) ) ;
#7118 = ORIENTED_EDGE ( 'NONE', *, *, #6716, .F. ) ;
#7119 = LINE ( 'NONE', #9931, #8630 ) ;
#7120 = EDGE_CURVE ( 'NONE', #6664, #9611, #3128, .T. ) ;
#7121 = DIRECTION ( 'NONE',  ( -0.000000000000000000, 1.000000000000000000, -0.000000000000000000 ) ) ;
#7122 = ORIENTED_EDGE ( 'NONE', *, *, #3296, .F. ) ;
#7123 = DIRECTION ( 'NONE',  ( -0.000000000000000000, -0.8916709834801178625, -0.4526840589413320126 ) ) ;
#7124 = VERTEX_POINT ( 'NONE', #2167 ) ;
#7125 = CARTESIAN_POINT ( 'NONE',  ( 0.000000000000000000, -21.74405275335753984, -5.984728032765188388 ) ) ;
#7126 = ORIENTED_EDGE ( 'NONE', *, *, #3099, .F. ) ;
#7127 = CARTESIAN_POINT ( 'NONE',  ( -25.00000000000000000, 0.000000000000000000, 0.000000000000000000 ) ) ;
#7128 = DIRECTION ( 'NONE',  ( 0.000000000000000000, 0.000000000000000000, 1.000000000000000000 ) ) ;
#7129 = ORIENTED_EDGE ( 'NONE', *, *, #12009, .F. ) ;
#7130 = DIRECTION ( 'NONE',  ( 1.000000000000000000, -0.000000000000000000, -0.000000000000000000 ) ) ;
#7131 = APPLICATION_CONTEXT ( 'automotive_design' ) ;
#7132 = FILL_AREA_STYLE_COLOUR ( '', #11964 ) ;
#7133 = DIRECTION ( 'NONE',  ( -1.000000000000000000, 4.770489558936236458E-18, 0.000000000000000000 ) ) ;
#7134 = CARTESIAN_POINT ( 'NONE',  ( 4.999999999999999112, 6.283573709965571297, -19.24938187143289881 ) ) ;
#7135 = DIRECTION ( 'NONE',  ( 0.000000000000000000, 0.000000000000000000, 1.000000000000000000 ) ) ;
#7136 = DIRECTION ( 'NONE',  ( -1.000000000000000000, -0.000000000000000000, 0.000000000000000000 ) ) ;
#7137 = VERTEX_POINT ( 'NONE', #8886 ) ;
#7138 = VERTEX_POINT ( 'NONE', #7812 ) ;
#7139 = EDGE_CURVE ( 'NONE', #9876, #8263, #6967, .T. ) ;
#7140 = DIRECTION ( 'NONE',  ( -0.000000000000000000, 1.000000000000000000, 0.000000000000000000 ) ) ;
#7141 = DIRECTION ( 'NONE',  ( 0.000000000000000000, -0.3826834323650773473, -0.9238795325112919565 ) ) ;
#7142 = VERTEX_POINT ( 'NONE', #11674 ) ;
#7143 = CYLINDRICAL_SURFACE ( 'NONE', #9087, 12.50000000000000000 ) ;
#7144 = EDGE_CURVE ( 'NONE', #10979, #3494, #5152, .T. ) ;
#7145 = ORIENTED_EDGE ( 'NONE', *, *, #8929, .T. ) ;
#7146 = DIRECTION ( 'NONE',  ( 0.000000000000000000, 0.000000000000000000, 1.000000000000000000 ) ) ;
#7147 = CARTESIAN_POINT ( 'NONE',  ( -15.00000000000000000, 40.00000000000000711, 0.000000000000000000 ) ) ;
#7148 = VERTEX_POINT ( 'NONE', #1299 ) ;
#7149 = CARTESIAN_POINT ( 'NONE',  ( 20.00000000000000000, 0.000000000000000000, 0.000000000000000000 ) ) ;
#7150 = LINE ( 'NONE', #1211, #7836 ) ;
#7151 = ORIENTED_EDGE ( 'NONE', *, *, #3739, .T. ) ;
#7152 = ADVANCED_FACE ( 'NONE', ( #1351 ), #11540, .F. ) ;
#7153 = DIRECTION ( 'NONE',  ( 0.000000000000000000, 0.000000000000000000, 1.000000000000000000 ) ) ;
#7154 = PLANE ( 'NONE',  #9612 ) ;
#7155 = VERTEX_POINT ( 'NONE', #5112 ) ;
#7156 = DIRECTION ( 'NONE',  ( 0.000000000000000000, 0.5000000000000011102, 0.8660254037844380415 ) ) ;
#7157 = EDGE_CURVE ( 'NONE', #2328, #5671, #2991, .T. ) ;
#7158 = ITEM_DEFINED_TRANSFORMATION ( 'NONE', 'NONE', #5244,  #6056 ) ;
#7159 = EDGE_CURVE ( 'NONE', #6849, #8668, #4161, .T. ) ;
#7160 = VERTEX_POINT ( 'NONE', #10794 ) ;
#7161 = EDGE_CURVE ( 'NONE', #3985, #3572, #4961, .T. ) ;
#7162 = LINE ( 'NONE', #3404, #4774 ) ;
#7163 = CIRCLE ( 'NONE', #10943, 7.200000000007204193 ) ;
#7164 = DIRECTION ( 'NONE',  ( -1.000000000000000000, -0.000000000000000000, 0.000000000000000000 ) ) ;
#7165 = DIRECTION ( 'NONE',  ( 0.000000000000000000, 0.000000000000000000, -1.000000000000000000 ) ) ;
#7166 = AXIS2_PLACEMENT_3D ( 'NONE', #5175, #5940, #2300 ) ;
#7167 = CONICAL_SURFACE ( 'NONE', #2765, 2.041999999999999815, 1.047197551196591858 ) ;
#7168 = FACE_OUTER_BOUND ( 'NONE', #4870, .T. ) ;
#7169 = DIRECTION ( 'NONE',  ( 0.000000000000000000, 1.000000000000000000, 3.614007241614734605E-15 ) ) ;
#7170 = VERTEX_POINT ( 'NONE', #6118 ) ;
#7171 = EDGE_CURVE ( 'NONE', #12241, #4691, #3248, .T. ) ;
#7172 = CARTESIAN_POINT ( 'NONE',  ( 2.500000000000000000, 1.178949249685213863, -2.042000000000001148 ) ) ;
#7173 = EDGE_LOOP ( 'NONE', ( #6402, #234, #3318, #11096 ) ) ;
#7174 = DIRECTION ( 'NONE',  ( 1.000000000000000000, 0.000000000000000000, 0.000000000000000000 ) ) ;
#7175 = ORIENTED_EDGE ( 'NONE', *, *, #712, .F. ) ;
#7177 = DIRECTION ( 'NONE',  ( 1.000000000000000000, 0.000000000000000000, 0.000000000000000000 ) ) ;
#7176 = CIRCLE ( 'NONE', #6573, 2.149999999999999023 ) ;
#7178 = CIRCLE ( 'NONE', #5374, 27.00000000002699707 ) ;
#7179 = DIRECTION ( 'NONE',  ( 1.000000000000000000, 0.000000000000000000, 0.000000000000000000 ) ) ;
#7180 = VERTEX_POINT ( 'NONE', #3070 ) ;
#7181 = CARTESIAN_POINT ( 'NONE',  ( 4.999999999999999112, -8.035066368449101049, -14.88411597386737562 ) ) ;
#7182 = AXIS2_PLACEMENT_3D ( 'NONE', #1156, #8800, #5731 ) ;
#7183 = AXIS2_PLACEMENT_3D ( 'NONE', #11479, #10543, #6620 ) ;
#7184 = VERTEX_POINT ( 'NONE', #8995 ) ;
#7185 = ADVANCED_FACE ( 'NONE', ( #1118 ), #9878, .T. ) ;
#7186 = ADVANCED_FACE ( 'NONE', ( #4165 ), #9749, .F. ) ;
#7187 = AXIS2_PLACEMENT_3D ( 'NONE', #7923, #3164, #6106 ) ;
#7188 = CARTESIAN_POINT ( 'NONE',  ( 0.000000000000000000, 14.46592441914986082, -15.22291137398907068 ) ) ;
#7189 = ORIENTED_EDGE ( 'NONE', *, *, #8386, .T. ) ;
#7190 = CARTESIAN_POINT ( 'NONE',  ( -31.74999999999995737, 0.000000000000000000, 0.000000000000000000 ) ) ;
#7191 = ORIENTED_EDGE ( 'NONE', *, *, #1076, .T. ) ;
#7192 = DIRECTION ( 'NONE',  ( 0.000000000000000000, 0.000000000000000000, 1.000000000000000000 ) ) ;
#7193 = AXIS2_PLACEMENT_3D ( 'NONE', #12081, #3532, #5346 ) ;
#7194 =( GEOMETRIC_REPRESENTATION_CONTEXT ( 3 ) GLOBAL_UNCERTAINTY_ASSIGNED_CONTEXT ( ( #9542 ) ) GLOBAL_UNIT_ASSIGNED_CONTEXT ( ( #10397, #7670, #1771 ) ) REPRESENTATION_CONTEXT ( 'NONE', 'WORKASPACE' ) );
#7195 = CARTESIAN_POINT ( 'NONE',  ( -33.00000000000000000, 0.000000000000000000, 0.000000000000000000 ) ) ;
#7196 = CARTESIAN_POINT ( 'NONE',  ( -1.400000000000000133, 0.000000000000000000, 0.000000000000000000 ) ) ;
#7197 = DIRECTION ( 'NONE',  ( 1.000000000000000000, -0.000000000000000000, -0.000000000000000000 ) ) ;
#7198 = DIRECTION ( 'NONE',  ( 0.000000000000000000, 0.000000000000000000, -1.000000000000000000 ) ) ;
#7199 = CARTESIAN_POINT ( 'NONE',  ( 5.000000000000000888, 0.000000000000000000, 0.000000000000000000 ) ) ;
#7200 = VECTOR ( 'NONE', #4086, 1000.000000000000000 ) ;
#7201 = ORIENTED_EDGE ( 'NONE', *, *, #128, .T. ) ;
#7202 = ORIENTED_EDGE ( 'NONE', *, *, #9401, .F. ) ;
#7203 = CARTESIAN_POINT ( 'NONE',  ( 70.79898987322334847, 3.500000000000001332, -38.49999999999998579 ) ) ;
#7204 = CARTESIAN_POINT ( 'NONE',  ( 4.999999999999999112, -0.4834863907624570856, -16.90755573046746463 ) ) ;
#7205 = AXIS2_PLACEMENT_3D ( 'NONE', #930, #6820, #1120 ) ;
#7206 = ORIENTED_EDGE ( 'NONE', *, *, #8716, .T. ) ;
#7207 = CARTESIAN_POINT ( 'NONE',  ( -38.00000000000000000, 0.000000000000000000, 0.000000000000000000 ) ) ;
#7208 = ORIENTED_EDGE ( 'NONE', *, *, #4388, .T. ) ;
#7209 = CARTESIAN_POINT ( 'NONE',  ( -1.399999999999998579, 9.184850993605147944E-16, 7.500000000000000000 ) ) ;
#7210 = CIRCLE ( 'NONE', #3409, 5.000000000000004441 ) ;
#7211 = CIRCLE ( 'NONE', #2015, 7.500000000000000000 ) ;
#7212 = ORIENTED_EDGE ( 'NONE', *, *, #6088, .F. ) ;
#7213 = VECTOR ( 'NONE', #45, 1000.000000000000114 ) ;
#7214 = DIRECTION ( 'NONE',  ( 0.000000000000000000, 0.000000000000000000, 1.000000000000000000 ) ) ;
#7215 = CARTESIAN_POINT ( 'NONE',  ( 0.000000000000000000, 0.000000000000000000, 0.000000000000000000 ) ) ;
#7216 = EDGE_CURVE ( 'NONE', #3527, #7793, #413, .T. ) ;
#7217 = SHAPE_REPRESENTATION ( 'spool', ( #6056 ), #10046 ) ;
#7218 = CARTESIAN_POINT ( 'NONE',  ( 15.00000000000000355, 44.00000000000001421, 0.000000000000000000 ) ) ;
#7219 = DIRECTION ( 'NONE',  ( -1.000000000000000000, -0.000000000000000000, -0.000000000000000000 ) ) ;
#7220 = VERTEX_POINT ( 'NONE', #4928 ) ;
#7221 = CARTESIAN_POINT ( 'NONE',  ( 1.600000000000000089, 0.000000000000000000, 2.700000000000000178 ) ) ;
#7222 = DIRECTION ( 'NONE',  ( 1.000000000000000000, -0.000000000000000000, -0.000000000000000000 ) ) ;
#7223 = AXIS2_PLACEMENT_3D ( 'NONE', #3537, #5593, #4668 ) ;
#7224 = AXIS2_PLACEMENT_3D ( 'NONE', #6232, #10857, #10049 ) ;
#7225 = EDGE_LOOP ( 'NONE', ( #2835, #9090, #12051, #2721 ) ) ;
#7226 = DIRECTION ( 'NONE',  ( -1.000000000000000000, -0.000000000000000000, 0.000000000000000000 ) ) ;
#7227 = AXIS2_PLACEMENT_3D ( 'NONE', #402, #4222, #11846 ) ;
#7228 = EDGE_LOOP ( 'NONE', ( #10505, #6770, #11101, #6272 ) ) ;
#7229 = AXIS2_PLACEMENT_3D ( 'NONE', #9627, #1060, #8808 ) ;
#7230 = EDGE_CURVE ( 'NONE', #3807, #12064, #3574, .T. ) ;
#7231 = CARTESIAN_POINT ( 'NONE',  ( 42.00000000000000000, -7.000000000000004441, -41.99999999999998579 ) ) ;
#7232 =( GEOMETRIC_REPRESENTATION_CONTEXT ( 3 ) GLOBAL_UNCERTAINTY_ASSIGNED_CONTEXT ( ( #2762 ) ) GLOBAL_UNIT_ASSIGNED_CONTEXT ( ( #8513, #7707, #936 ) ) REPRESENTATION_CONTEXT ( 'NONE', 'WORKASPACE' ) );
#7233 = AXIS2_PLACEMENT_3D ( 'NONE', #2713, #6481, #8415 ) ;
#7234 = CIRCLE ( 'NONE', #11608, 4.799999999999998934 ) ;
#7235 = DIRECTION ( 'NONE',  ( 0.000000000000000000, -0.4999999999999993894, 0.8660254037844389297 ) ) ;
#7236 = CARTESIAN_POINT ( 'NONE',  ( 4.999999999999999112, 0.000000000000000000, 0.000000000000000000 ) ) ;
#7237 = EDGE_CURVE ( 'NONE', #10134, #3460, #7163, .T. ) ;
#7238 = AXIS2_PLACEMENT_3D ( 'NONE', #7787, #9483, #11578 ) ;
#7239 = AXIS2_PLACEMENT_3D ( 'NONE', #4197, #7962, #7092 ) ;
#7240 = DIRECTION ( 'NONE',  ( 0.000000000000000000, 0.4999999999999948930, 0.8660254037844414832 ) ) ;
#7242 = ADVANCED_FACE ( 'NONE', ( #2534 ), #9181, .T. ) ;
#7241 = CARTESIAN_POINT ( 'NONE',  ( 37.00000000000000711, 1.456773409934505593E-31, -41.99999999999998579 ) ) ;
#7243 = EDGE_LOOP ( 'NONE', ( #3211, #9374, #2083, #11611 ) ) ;
#7244 = CYLINDRICAL_SURFACE ( 'NONE', #4843, 7.500000000000000000 ) ;
#7245 = ORIENTED_EDGE ( 'NONE', *, *, #408, .F. ) ;
#7246 = CARTESIAN_POINT ( 'NONE',  ( 0.000000000000000000, 0.000000000000000000, 0.000000000000000000 ) ) ;
#7247 = VERTEX_POINT ( 'NONE', #6425 ) ;
#7248 =( GEOMETRIC_REPRESENTATION_CONTEXT ( 3 ) GLOBAL_UNCERTAINTY_ASSIGNED_CONTEXT ( ( #11388 ) ) GLOBAL_UNIT_ASSIGNED_CONTEXT ( ( #12161, #10545, #985 ) ) REPRESENTATION_CONTEXT ( 'NONE', 'WORKASPACE' ) );
#7249 = AXIS2_PLACEMENT_3D ( 'NONE', #8400, #8334, #10264 ) ;
#7250 = CARTESIAN_POINT ( 'NONE',  ( 2.499999999999999556, -14.46592441914974714, 15.22291137398917193 ) ) ;
#7251 = AXIS2_PLACEMENT_3D ( 'NONE', #7572, #4751, #7645 ) ;
#7252 = PRODUCT_DEFINITION_SHAPE ( 'NONE', 'NONE',  #12362 ) ;
#7253 = VECTOR ( 'NONE', #12190, 1000.000000000000000 ) ;
#7254 = DIRECTION ( 'NONE',  ( 0.000000000000000000, 0.000000000000000000, -1.000000000000000000 ) ) ;
#7255 = ORIENTED_EDGE ( 'NONE', *, *, #9786, .F. ) ;
#7256 = CARTESIAN_POINT ( 'NONE',  ( 4.999999999999999112, -14.88411597386734897, 8.035066368449154339 ) ) ;
#7257 = VECTOR ( 'NONE', #1134, 1000.000000000000000 ) ;
#7258 = EDGE_CURVE ( 'NONE', #5539, #7138, #4292, .T. ) ;
#7259 = AXIS2_PLACEMENT_3D ( 'NONE', #1780, #9417, #6676 ) ;
#7260 = VERTEX_POINT ( 'NONE', #5303 ) ;
#7261 = AXIS2_PLACEMENT_3D ( 'NONE', #2621, #8319, #5508 ) ;
#7262 = CARTESIAN_POINT ( 'NONE',  ( 1.600000000000000089, 0.000000000000000000, 0.000000000000000000 ) ) ;
#7263 = VERTEX_POINT ( 'NONE', #3358 ) ;
#7264 = DIRECTION ( 'NONE',  ( -1.000000000000000000, 0.000000000000000000, 0.000000000000000000 ) ) ;
#7265 = ORIENTED_EDGE ( 'NONE', *, *, #9916, .F. ) ;
#7266 = FACE_OUTER_BOUND ( 'NONE', #1726, .T. ) ;
#7267 = EDGE_CURVE ( 'NONE', #8289, #3971, #3176, .T. ) ;
#7268 = CIRCLE ( 'NONE', #4062, 9.600000000009600853 ) ;
#7269 = ADVANCED_FACE ( 'NONE', ( #6357 ), #10235, .T. ) ;
#7270 = FACE_OUTER_BOUND ( 'NONE', #2023, .T. ) ;
#7271 = DIRECTION ( 'NONE',  ( -1.000000000000000000, 0.000000000000000000, 0.000000000000000000 ) ) ;
#7272 = FACE_OUTER_BOUND ( 'NONE', #253, .T. ) ;
#7273 = DIRECTION ( 'NONE',  ( 1.000000000000000000, -0.000000000000000000, -0.000000000000000000 ) ) ;
#7274 = CARTESIAN_POINT ( 'NONE',  ( 4.999999999999999112, -22.05152472667118957, -15.57980286237495626 ) ) ;
#7275 = ORIENTED_EDGE ( 'NONE', *, *, #11194, .F. ) ;
#7276 = ORIENTED_EDGE ( 'NONE', *, *, #3250, .T. ) ;
#7277 = CARTESIAN_POINT ( 'NONE',  ( 0.2500000000000002220, 0.000000000000000000, 4.000000000000000000 ) ) ;
#7278 = AXIS2_PLACEMENT_3D ( 'NONE', #12278, #12215, #10228 ) ;
#7279 = DIRECTION ( 'NONE',  ( -1.000000000000000000, 0.000000000000000000, 0.000000000000000000 ) ) ;
#7280 = EDGE_LOOP ( 'NONE', ( #9283, #2558, #7683, #8728 ) ) ;
#7281 = DIRECTION ( 'NONE',  ( 0.000000000000000000, -1.000000000000000000, 0.000000000000000000 ) ) ;
#7282 = ORIENTED_EDGE ( 'NONE', *, *, #11525, .F. ) ;
#7283 = CARTESIAN_POINT ( 'NONE',  ( 0.000000000000000000, 9.168210874537578547, 18.05452603534168787 ) ) ;
#7284 = VECTOR ( 'NONE', #4852, 1000.000000000000000 ) ;
#7285 = DIRECTION ( 'NONE',  ( 1.000000000000000000, 0.000000000000000000, 0.000000000000000000 ) ) ;
#7286 = DIRECTION ( 'NONE',  ( -1.000000000000000000, -0.000000000000000000, -0.000000000000000000 ) ) ;
#7287 = PLANE ( 'NONE',  #3062 ) ;
#7288 = CARTESIAN_POINT ( 'NONE',  ( 42.00000000000000000, 3.792354139917828437, 2.942456469932579921 ) ) ;
#7289 = ORIENTED_EDGE ( 'NONE', *, *, #11505, .F. ) ;
#7290 = FACE_OUTER_BOUND ( 'NONE', #6101, .T. ) ;
#7291 = CARTESIAN_POINT ( 'NONE',  ( 0.000000000000000000, 46.00000000000001421, -41.99999999999999289 ) ) ;
#7292 = ORIENTED_EDGE ( 'NONE', *, *, #3873, .F. ) ;
#7293 = DIRECTION ( 'NONE',  ( 1.000000000000000000, -0.000000000000000000, -0.000000000000000000 ) ) ;
#7294 = ITEM_DEFINED_TRANSFORMATION ( 'NONE', 'NONE', #6250,  #6056 ) ;
#7295 = AXIS2_PLACEMENT_3D ( 'NONE', #7667, #4709, #11567 ) ;
#7296 = EDGE_LOOP ( 'NONE', ( #8622, #2379, #8527, #7484 ) ) ;
#7297 = DIRECTION ( 'NONE',  ( 0.000000000000000000, 1.000000000000000000, -1.287488025362403787E-15 ) ) ;
#7298 = CARTESIAN_POINT ( 'NONE',  ( 4.999999999999999112, 0.000000000000000000, 0.000000000000000000 ) ) ;
#7299 = LINE ( 'NONE', #4338, #5822 ) ;
#7300 = VECTOR ( 'NONE', #11805, 1000.000000000000000 ) ;
#7301 = PLANE ( 'NONE',  #422 ) ;
#7302 = CYLINDRICAL_SURFACE ( 'NONE', #4034, 20.24900000002024569 ) ;
#7303 = ORIENTED_EDGE ( 'NONE', *, *, #2613, .F. ) ;
#7304 = CYLINDRICAL_SURFACE ( 'NONE', #453, 9.600000000009600853 ) ;
#7305 = ORIENTED_EDGE ( 'NONE', *, *, #8217, .T. ) ;
#7306 = CARTESIAN_POINT ( 'NONE',  ( 16.55500000000001393, 0.000000000000000000, 0.000000000000000000 ) ) ;
#7307 = ADVANCED_FACE ( 'NONE', ( #2598 ), #6560, .T. ) ;
#7308 =( NAMED_UNIT ( * ) SI_UNIT ( $, .STERADIAN. ) SOLID_ANGLE_UNIT ( ) );
#7309 = EDGE_LOOP ( 'NONE', ( #9051, #11389, #9704, #8276 ) ) ;
#7310 = DIRECTION ( 'NONE',  ( 1.000000000000000000, -0.000000000000000000, -0.000000000000000000 ) ) ;
#7311 = APPLICATION_CONTEXT ( 'automotive_design' ) ;
#7312 = EDGE_CURVE ( 'NONE', #7148, #8658, #6773, .T. ) ;
#7313 = CIRCLE ( 'NONE', #1911, 4.000000000000000000 ) ;
#7314 = DIRECTION ( 'NONE',  ( 0.000000000000000000, 0.000000000000000000, 1.000000000000000000 ) ) ;
#7315 = ORIENTED_EDGE ( 'NONE', *, *, #343, .F. ) ;
#7316 = CARTESIAN_POINT ( 'NONE',  ( 46.00000000000000000, -3.499999999999998668, -38.49999999999998579 ) ) ;
#7317 = ORIENTED_EDGE ( 'NONE', *, *, #10006, .T. ) ;
#7318 = DIRECTION ( 'NONE',  ( 1.000000000000000000, 0.000000000000000000, 0.000000000000000000 ) ) ;
#7319 = ORIENTED_EDGE ( 'NONE', *, *, #11638, .T. ) ;
#7320 = LINE ( 'NONE', #1684, #10097 ) ;
#7321 = ADVANCED_FACE ( 'NONE', ( #538 ), #5426, .T. ) ;
#7323 = ORIENTED_EDGE ( 'NONE', *, *, #4876, .T. ) ;
#7322 = EDGE_CURVE ( 'NONE', #10639, #1934, #4415, .T. ) ;
#7324 = DIRECTION ( 'NONE',  ( -1.000000000000000000, 0.000000000000000000, 0.000000000000000000 ) ) ;
#7325 = EDGE_CURVE ( 'NONE', #4584, #3417, #764, .T. ) ;
#7326 = CARTESIAN_POINT ( 'NONE',  ( 4.999999999999999112, -13.09267581720863127, -5.622796541391703151 ) ) ;
#7327 = DIRECTION ( 'NONE',  ( 1.000000000000000000, 0.000000000000000000, -0.000000000000000000 ) ) ;
#7328 = CARTESIAN_POINT ( 'NONE',  ( 33.00000000000000000, 0.000000000000000000, 0.000000000000000000 ) ) ;
#7329 = FACE_OUTER_BOUND ( 'NONE', #6707, .T. ) ;
#7330 = ORIENTED_EDGE ( 'NONE', *, *, #3973, .T. ) ;
#7331 = ORIENTED_EDGE ( 'NONE', *, *, #9060, .T. ) ;
#7332 = DIRECTION ( 'NONE',  ( -1.000000000000000000, 0.000000000000000000, 0.000000000000000000 ) ) ;
#7333 = EDGE_CURVE ( 'NONE', #4657, #4612, #7176, .T. ) ;
#7334 = CARTESIAN_POINT ( 'NONE',  ( -2.595115354961444076, -7.673029147243174641, -1.000000000000000000 ) ) ;
#7335 = VERTEX_POINT ( 'NONE', #673 ) ;
#7336 = CARTESIAN_POINT ( 'NONE',  ( 42.00000000000000000, 5.000000000000004441, -41.99999999999998579 ) ) ;
#7337 = ORIENTED_EDGE ( 'NONE', *, *, #3118, .F. ) ;
#7338 = DIRECTION ( 'NONE',  ( -0.000000000000000000, 1.000000000000000000, -0.000000000000000000 ) ) ;
#7339 = FACE_OUTER_BOUND ( 'NONE', #10423, .T. ) ;
#7340 = CARTESIAN_POINT ( 'NONE',  ( 2.499999999999999556, -5.950465759859009829, 20.13931372320386259 ) ) ;
#7341 = DIRECTION ( 'NONE',  ( -0.000000000000000000, 1.000000000000000000, 0.000000000000000000 ) ) ;
#7342 = DIRECTION ( 'NONE',  ( 0.000000000000000000, 0.000000000000000000, 1.000000000000000000 ) ) ;
#7343 = ORIENTED_EDGE ( 'NONE', *, *, #8147, .T. ) ;
#7344 = CARTESIAN_POINT ( 'NONE',  ( -36.00000000000000711, 0.000000000000000000, 0.000000000000000000 ) ) ;
#7345 = EDGE_CURVE ( 'NONE', #1358, #6331, #8304, .T. ) ;
#7346 = CARTESIAN_POINT ( 'NONE',  ( 26.00000000000000355, 0.000000000000000000, -19.99999999999998934 ) ) ;
#7347 = VERTEX_POINT ( 'NONE', #7361 ) ;
#7348 = ORIENTED_EDGE ( 'NONE', *, *, #3674, .T. ) ;
#7349 = CARTESIAN_POINT ( 'NONE',  ( 0.000000000000000000, 6.123233995736766282E-16, -5.000000000000000000 ) ) ;
#7350 = CARTESIAN_POINT ( 'NONE',  ( 2.499999999999999556, 14.46592441914986082, -15.22291137398907068 ) ) ;
#7351 = FACE_OUTER_BOUND ( 'NONE', #12060, .T. ) ;
#7352 = DIRECTION ( 'NONE',  ( -1.000000000000000000, -0.000000000000000000, -0.000000000000000000 ) ) ;
#7353 = LINE ( 'NONE', #5532, #4815 ) ;
#7354 = EDGE_LOOP ( 'NONE', ( #4993, #12281, #2423, #2929 ) ) ;
#7355 = CARTESIAN_POINT ( 'NONE',  ( 37.00000000000000711, 5.702959862028875726, -38.29645456189778940 ) ) ;
#7356 = ORIENTED_EDGE ( 'NONE', *, *, #5995, .T. ) ;
#7357 = SURFACE_SIDE_STYLE ('',( #12144 ) ) ;
#7358 = CARTESIAN_POINT ( 'NONE',  ( 0.000000000000000000, 0.000000000000000000, 0.000000000000000000 ) ) ;
#7359 = ORIENTED_EDGE ( 'NONE', *, *, #10243, .F. ) ;
#7360 = LINE ( 'NONE', #6304, #11803 ) ;
#7361 = CARTESIAN_POINT ( 'NONE',  ( 4.999999999999999112, 11.41582255376084909, -8.527191590520953213 ) ) ;
#7362 = AXIS2_PLACEMENT_3D ( 'NONE', #6186, #685, #5503 ) ;
#7363 = CIRCLE ( 'NONE', #1974, 2.149999999999999023 ) ;
#7364 = VERTEX_POINT ( 'NONE', #8251 ) ;
#7365 = CARTESIAN_POINT ( 'NONE',  ( 46.00000000000000000, 1.444447458290426890E-31, -41.99999999999998579 ) ) ;
#7366 = ADVANCED_FACE ( 'NONE', ( #11161 ), #3490, .T. ) ;
#7367 = EDGE_CURVE ( 'NONE', #8107, #10292, #377, .T. ) ;
#7368 = ORIENTED_EDGE ( 'NONE', *, *, #2816, .F. ) ;
#7369 = DIRECTION ( 'NONE',  ( 1.000000000000000000, 0.000000000000000000, 0.000000000000000000 ) ) ;
#7370 = VECTOR ( 'NONE', #6633, 1000.000000000000000 ) ;
#7371 = ORIENTED_EDGE ( 'NONE', *, *, #12169, .F. ) ;
#7372 = CIRCLE ( 'NONE', #5167, 5.000000000000000000 ) ;
#7373 = DIRECTION ( 'NONE',  ( 0.000000000000000000, 0.8772744497699204169, 0.4799891038147465205 ) ) ;
#7374 = ORIENTED_EDGE ( 'NONE', *, *, #4739, .F. ) ;
#7375 = DIRECTION ( 'NONE',  ( 1.000000000000000000, 0.000000000000000000, 0.000000000000000000 ) ) ;
#7376 = AXIS2_PLACEMENT_3D ( 'NONE', #706, #10146, #1580 ) ;
#7377 = VECTOR ( 'NONE', #8500, 1000.000000000000000 ) ;
#7378 = CARTESIAN_POINT ( 'NONE',  ( 0.2500000000000002220, 0.000000000000000000, 0.000000000000000000 ) ) ;
#7379 = EDGE_CURVE ( 'NONE', #10072, #4240, #2349, .T. ) ;
#7380 = CONICAL_SURFACE ( 'NONE', #8981, 2.055000000000000160, 0.7853981633974633780 ) ;
#7381 = EDGE_CURVE ( 'NONE', #4485, #504, #1172, .T. ) ;
#7382 = DIRECTION ( 'NONE',  ( -1.000000000000000000, -0.000000000000000000, -0.000000000000000000 ) ) ;
#7383 = CARTESIAN_POINT ( 'NONE',  ( 36.00000000000000000, 40.00000000000000711, 20.00000000000001066 ) ) ;
#7384 = EDGE_CURVE ( 'NONE', #231, #3450, #1489, .T. ) ;
#7385 = VERTEX_POINT ( 'NONE', #8429 ) ;
#7386 = ORIENTED_EDGE ( 'NONE', *, *, #4487, .T. ) ;
#7387 = CARTESIAN_POINT ( 'NONE',  ( 4.999999999999999112, 0.000000000000000000, 0.000000000000000000 ) ) ;
#7388 = DIRECTION ( 'NONE',  ( 0.000000000000000000, 0.000000000000000000, 1.000000000000000000 ) ) ;
#7389 = CIRCLE ( 'NONE', #8387, 9.600000000009599077 ) ;
#7390 = PLANE ( 'NONE',  #10479 ) ;
#7391 = VECTOR ( 'NONE', #3194, 1000.000000000000000 ) ;
#7392 = VERTEX_POINT ( 'NONE', #12223 ) ;
#7393 = DIRECTION ( 'NONE',  ( 0.000000000000000000, 0.000000000000000000, -1.000000000000000000 ) ) ;
#7394 = AXIS2_PLACEMENT_3D ( 'NONE', #3443, #5071, #3198 ) ;
#7395 = VECTOR ( 'NONE', #10047, 1000.000000000000000 ) ;
#7396 = CARTESIAN_POINT ( 'NONE',  ( 0.000000000000000000, 16.90755573046746107, 6.716513609244568528 ) ) ;
#7397 = DIRECTION ( 'NONE',  ( -1.000000000000000000, -0.000000000000000000, -0.000000000000000000 ) ) ;
#7398 = EDGE_LOOP ( 'NONE', ( #2560, #8539, #7303, #1336 ) ) ;
#7399 = CIRCLE ( 'NONE', #603, 6.500000000000000888 ) ;
#7400 = FACE_BOUND ( 'NONE', #2764, .T. ) ;
#7401 = DIRECTION ( 'NONE',  ( 0.000000000000000000, 0.000000000000000000, -1.000000000000000000 ) ) ;
#7402 = PRODUCT_DEFINITION ( 'UNKNOWN', '', #3251, #4263 ) ;
#7403 = ORIENTED_EDGE ( 'NONE', *, *, #5949, .T. ) ;
#7404 = DIRECTION ( 'NONE',  ( -1.000000000000000000, -0.000000000000000000, 0.000000000000000000 ) ) ;
#7405 = DIRECTION ( 'NONE',  ( -1.000000000000000000, -0.000000000000000000, -0.000000000000000000 ) ) ;
#7406 = EDGE_LOOP ( 'NONE', ( #3223, #12248, #3955, #1381 ) ) ;
#7407 = VERTEX_POINT ( 'NONE', #9360 ) ;
#7408=STYLED_ITEM('',(#12412),#8493);
#7409 = CIRCLE ( 'NONE', #808, 0.7499999999999997780 ) ;
#7410 = ADVANCED_FACE ( 'NONE', ( #1790, #5600, #1925 ), #6492, .F. ) ;
#7411 = ADVANCED_FACE ( 'NONE', ( #4729 ), #5672, .T. ) ;
#7412 = DIRECTION ( 'NONE',  ( 0.000000000000000000, 0.000000000000000000, 1.000000000000000000 ) ) ;
#7413 = CYLINDRICAL_SURFACE ( 'NONE', #11195, 20.24900000002024569 ) ;
#7414 = DIRECTION ( 'NONE',  ( 0.000000000000000000, 0.000000000000000000, 1.000000000000000000 ) ) ;
#7415 = CARTESIAN_POINT ( 'NONE',  ( 0.000000000000000000, -5.984728032764810024, -21.74405275335764287 ) ) ;
#7416 = CIRCLE ( 'NONE', #10602, 5.000000000000000000 ) ;
#7417 = CIRCLE ( 'NONE', #416, 5.000000000000000000 ) ;
#7418 = ORIENTED_EDGE ( 'NONE', *, *, #12104, .F. ) ;
#7419 = VERTEX_POINT ( 'NONE', #7546 ) ;
#7420 = CIRCLE ( 'NONE', #6032, 2.000000000000000000 ) ;
#7421 = LINE ( 'NONE', #1722, #64 ) ;
#7422 = AXIS2_PLACEMENT_3D ( 'NONE', #8413, #3595, #766 ) ;
#7423 = ORIENTED_EDGE ( 'NONE', *, *, #4875, .F. ) ;
#7424 = DIRECTION ( 'NONE',  ( 0.000000000000000000, 0.000000000000000000, 1.000000000000000000 ) ) ;
#7425 = EDGE_LOOP ( 'NONE', ( #6739, #4727, #4017, #2141 ) ) ;
#7426 = DIRECTION ( 'NONE',  ( 0.9995235871707960351, -0.03086419753086420970, 0.000000000000000000 ) ) ;
#7427 = CARTESIAN_POINT ( 'NONE',  ( 4.999999999999999112, -16.90755573046746463, 0.4834863907625160939 ) ) ;
#7428 =( GEOMETRIC_REPRESENTATION_CONTEXT ( 3 ) GLOBAL_UNCERTAINTY_ASSIGNED_CONTEXT ( ( #9406 ) ) GLOBAL_UNIT_ASSIGNED_CONTEXT ( ( #71, #2125, #3136 ) ) REPRESENTATION_CONTEXT ( 'NONE', 'WORKASPACE' ) );
#7429 = VECTOR ( 'NONE', #46, 1000.000000000000000 ) ;
#7430 = AXIS2_PLACEMENT_3D ( 'NONE', #2317, #2445, #6271 ) ;
#7431 = CIRCLE ( 'NONE', #832, 5.000000000000004441 ) ;
#7432 = VECTOR ( 'NONE', #4455, 1000.000000000000000 ) ;
#7433 = EDGE_LOOP ( 'NONE', ( #6623, #4886, #5093, #12061, #8130, #11286, #10017, #5583 ) ) ;
#7434 = DIRECTION ( 'NONE',  ( 1.000000000000000000, 0.000000000000000000, 0.000000000000000000 ) ) ;
#7435 = VERTEX_POINT ( 'NONE', #3608 ) ;
#7436 = CARTESIAN_POINT ( 'NONE',  ( 0.000000000000000000, 2.357898499370433054, -1.951563910473907981E-15 ) ) ;
#7437 = AXIS2_PLACEMENT_3D ( 'NONE', #12209, #6412, #9240 ) ;
#7438 = VERTEX_POINT ( 'NONE', #6610 ) ;
#7439 = AXIS2_PLACEMENT_3D ( 'NONE', #7127, #6002, #9886 ) ;
#7440 = AXIS2_PLACEMENT_3D ( 'NONE', #10144, #1645, #1576 ) ;
#7441 = CARTESIAN_POINT ( 'NONE',  ( 0.000000000000000000, -8.035066368449308882, 14.88411597386726193 ) ) ;
#7442 = VERTEX_POINT ( 'NONE', #12337 ) ;
#7443 = CARTESIAN_POINT ( 'NONE',  ( 4.999999999999999112, -5.955107813822311691, -26.33508479058326657 ) ) ;
#7444 = EDGE_CURVE ( 'NONE', #9986, #2114, #3789, .T. ) ;
#7445 = ADVANCED_FACE ( 'NONE', ( #915 ), #10412, .T. ) ;
#7446 = AXIS2_PLACEMENT_3D ( 'NONE', #668, #3541, #12090 ) ;
#7447 = AXIS2_PLACEMENT_3D ( 'NONE', #12189, #10386, #9217 ) ;
#7448 = CARTESIAN_POINT ( 'NONE',  ( 0.000000000000000000, 16.90755573046745397, 0.4834863907628708102 ) ) ;
#7449 = CARTESIAN_POINT ( 'NONE',  ( 37.00000000000000711, -3.403685371105885427, -38.61548734756097190 ) ) ;
#7450 = DIRECTION ( 'NONE',  ( -1.000000000000000000, -0.000000000000000000, 0.000000000000000000 ) ) ;
#7451 = VERTEX_POINT ( 'NONE', #11411 ) ;
#7452 = EDGE_LOOP ( 'NONE', ( #5685, #9807, #9365, #2112, #4737, #1864, #1507, #9247, #6736, #1627, #8505, #10488 ) ) ;
#7453 = CARTESIAN_POINT ( 'NONE',  ( 37.00000000000000711, -0.8169585525225422362, -40.74199414808185793 ) ) ;
#7454 = SURFACE_SIDE_STYLE ('',( #2005 ) ) ;
#7455 = DIRECTION ( 'NONE',  ( -0.000000000000000000, -0.000000000000000000, -1.000000000000000000 ) ) ;
#7456 = AXIS2_PLACEMENT_3D ( 'NONE', #500, #4186, #11743 ) ;
#7457 = DIRECTION ( 'NONE',  ( -1.000000000000000000, -0.000000000000000000, -0.000000000000000000 ) ) ;
#7458 = EDGE_CURVE ( 'NONE', #11041, #3700, #10291, .T. ) ;
#7459 = VECTOR ( 'NONE', #7705, 1000.000000000000000 ) ;
#7460 = VERTEX_POINT ( 'NONE', #3732 ) ;
#7461 = CYLINDRICAL_SURFACE ( 'NONE', #428, 2.149999999999999023 ) ;
#7462 = EDGE_CURVE ( 'NONE', #8252, #11705, #982, .T. ) ;
#7463 = ADVANCED_FACE ( 'NONE', ( #780 ), #11289, .F. ) ;
#7464 = CARTESIAN_POINT ( 'NONE',  ( 0.000000000000000000, 0.5192545390863916310, -1.000000000000000000 ) ) ;
#7465 = AXIS2_PLACEMENT_3D ( 'NONE', #3941, #5353, #9305 ) ;
#7466 = ORIENTED_EDGE ( 'NONE', *, *, #4148, .F. ) ;
#7467 = CARTESIAN_POINT ( 'NONE',  ( 1.500000000000001332, 0.000000000000000000, -5.525000000000000355 ) ) ;
#7468 = FACE_OUTER_BOUND ( 'NONE', #5056, .T. ) ;
#7469 = ORIENTED_EDGE ( 'NONE', *, *, #119, .F. ) ;
#7470 = DIRECTION ( 'NONE',  ( -1.000000000000000000, 0.000000000000000000, -0.000000000000000000 ) ) ;
#7471 = LINE ( 'NONE', #2705, #11592 ) ;
#7472 = EDGE_LOOP ( 'NONE', ( #4257, #8916 ) ) ;
#7473 = CARTESIAN_POINT ( 'NONE',  ( 1.000000000000000000, 0.000000000000000000, 0.000000000000000000 ) ) ;
#7474 = EDGE_LOOP ( 'NONE', ( #11222, #11281, #10462, #524 ) ) ;
#7475 = ADVANCED_FACE ( 'NONE', ( #2784 ), #8977, .T. ) ;
#7476 = COLOUR_RGB ( '',0.8941176470588234615, 0.8941176470588234615, 0.8941176470588234615 ) ;
#7477 = EDGE_CURVE ( 'NONE', #12254, #2589, #12150, .T. ) ;
#7478 = EDGE_CURVE ( 'NONE', #5131, #7419, #10478, .T. ) ;
#7479 = CYLINDRICAL_SURFACE ( 'NONE', #1396, 21.00000000002100009 ) ;
#7480 = DIRECTION ( 'NONE',  ( -0.000000000000000000, 0.000000000000000000, 1.000000000000000000 ) ) ;
#7481 = DIRECTION ( 'NONE',  ( -1.000000000000000000, 0.000000000000000000, 0.000000000000000000 ) ) ;
#7482 = DIRECTION ( 'NONE',  ( 1.000000000000000000, 0.000000000000000000, 0.000000000000000000 ) ) ;
#7483 = ORIENTED_EDGE ( 'NONE', *, *, #1964, .T. ) ;
#7484 = ORIENTED_EDGE ( 'NONE', *, *, #4016, .F. ) ;
#7485 = AXIS2_PLACEMENT_3D ( 'NONE', #5524, #9344, #2464 ) ;
#7486 = DIRECTION ( 'NONE',  ( -1.000000000000000000, -0.000000000000000000, -0.000000000000000000 ) ) ;
#7487 = ORIENTED_EDGE ( 'NONE', *, *, #6947, .F. ) ;
#7488 = FACE_OUTER_BOUND ( 'NONE', #8100, .T. ) ;
#7489 = APPLICATION_PROTOCOL_DEFINITION ( 'draft international standard', 'automotive_design', 1998, #3073 ) ;
#7490 = EDGE_CURVE ( 'NONE', #1263, #4341, #7975, .T. ) ;
#7492 = ADVANCED_FACE ( 'NONE', ( #3469 ), #11139, .T. ) ;
#7491 = EDGE_LOOP ( 'NONE', ( #8033, #12018 ) ) ;
#7493 = CARTESIAN_POINT ( 'NONE',  ( 0.000000000000000000, 0.000000000000000000, -1.000000000000000000 ) ) ;
#7494 = DIRECTION ( 'NONE',  ( 0.000000000000000000, 0.000000000000000000, 1.000000000000000000 ) ) ;
#7495 = VECTOR ( 'NONE', #4940, 1000.000000000000000 ) ;
#7496 = ORIENTED_EDGE ( 'NONE', *, *, #11192, .T. ) ;
#7497 = DIRECTION ( 'NONE',  ( 0.000000000000000000, 0.000000000000000000, -1.000000000000000000 ) ) ;
#7498 = CARTESIAN_POINT ( 'NONE',  ( 0.000000000000000000, -4.916402349214440193, -20.41639017900864772 ) ) ;
#7499 = VERTEX_POINT ( 'NONE', #5521 ) ;
#7500 = DIRECTION ( 'NONE',  ( 0.000000000000000000, 0.000000000000000000, -1.000000000000000000 ) ) ;
#7501 = ORIENTED_EDGE ( 'NONE', *, *, #7384, .T. ) ;
#7502 = EDGE_CURVE ( 'NONE', #5859, #7184, #10763, .T. ) ;
#7503 = FACE_OUTER_BOUND ( 'NONE', #11566, .T. ) ;
#7504 = ADVANCED_BREP_SHAPE_REPRESENTATION ( '', ( #280, #6056 ), #10030 ) ;
#7505 = ORIENTED_EDGE ( 'NONE', *, *, #1789, .T. ) ;
#7506 = CARTESIAN_POINT ( 'NONE',  ( 1.600000000000000089, 3.306546357697853733E-16, -2.700000000000000178 ) ) ;
#7507 = CARTESIAN_POINT ( 'NONE',  ( 4.999999999999999112, 4.576198416197620134, -26.60936692326685460 ) ) ;
#7508 = DIRECTION ( 'NONE',  ( 0.000000000000000000, 0.000000000000000000, -1.000000000000000000 ) ) ;
#7509 = DIRECTION ( 'NONE',  ( 0.000000000000000000, 0.000000000000000000, -1.000000000000000000 ) ) ;
#7510 = ORIENTED_EDGE ( 'NONE', *, *, #6010, .T. ) ;
#7511 = ORIENTED_EDGE ( 'NONE', *, *, #10379, .F. ) ;
#7512 = CARTESIAN_POINT ( 'NONE',  ( 0.000000000000000000, 0.000000000000000000, -1.000000000000000000 ) ) ;
#7513 = DIRECTION ( 'NONE',  ( 0.000000000000000000, 0.000000000000000000, 1.000000000000000000 ) ) ;
#7514 = DIRECTION ( 'NONE',  ( 0.000000000000000000, 0.000000000000000000, 1.000000000000000000 ) ) ;
#7515 = ORIENTED_EDGE ( 'NONE', *, *, #1656, .F. ) ;
#7516 = CARTESIAN_POINT ( 'NONE',  ( 15.00000000000000355, 30.00000000000000711, 1.999999999999998224 ) ) ;
#7517 = DIRECTION ( 'NONE',  ( 1.000000000000000000, 0.000000000000000000, 0.000000000000000000 ) ) ;
#7518 = CYLINDRICAL_SURFACE ( 'NONE', #12177, 14.24900000001425227 ) ;
#7519 = EDGE_CURVE ( 'NONE', #4854, #5131, #10037, .T. ) ;
#7520 = ORIENTED_EDGE ( 'NONE', *, *, #8691, .F. ) ;
#7521 = DIRECTION ( 'NONE',  ( -1.000000000000000000, -0.000000000000000000, -0.000000000000000000 ) ) ;
#7522 = FACE_OUTER_BOUND ( 'NONE', #3619, .T. ) ;
#7523 = ORIENTED_EDGE ( 'NONE', *, *, #9163, .F. ) ;
#7524 = ADVANCED_FACE ( 'NONE', ( #11085 ), #10206, .T. ) ;
#7525 = CARTESIAN_POINT ( 'NONE',  ( 45.00000000000000000, 0.000000000000000000, 0.000000000000000000 ) ) ;
#7526 = CARTESIAN_POINT ( 'NONE',  ( 0.000000000000000000, 0.000000000000000000, 0.000000000000000000 ) ) ;
#7527 = ORIENTED_EDGE ( 'NONE', *, *, #2819, .F. ) ;
#7528 = PLANE ( 'NONE',  #2288 ) ;
#7529 = ORIENTED_EDGE ( 'NONE', *, *, #7613, .T. ) ;
#7530 =( NAMED_UNIT ( * ) SI_UNIT ( $, .STERADIAN. ) SOLID_ANGLE_UNIT ( ) );
#7531 = DIRECTION ( 'NONE',  ( 0.000000000000000000, 0.000000000000000000, 1.000000000000000000 ) ) ;
#7532 = DIRECTION ( 'NONE',  ( 0.000000000000000000, 0.000000000000000000, 1.000000000000000000 ) ) ;
#7533 = EDGE_CURVE ( 'NONE', #403, #6433, #7773, .T. ) ;
#7534 = DIRECTION ( 'NONE',  ( -1.000000000000000000, -0.000000000000000000, 0.000000000000000000 ) ) ;
#7535 = DIRECTION ( 'NONE',  ( -1.000000000000000000, -0.000000000000000000, -0.000000000000000000 ) ) ;
#7536 = VERTEX_POINT ( 'NONE', #1650 ) ;
#7538 = ADVANCED_FACE ( 'NONE', ( #12126 ), #5399, .F. ) ;
#7537 = ORIENTED_EDGE ( 'NONE', *, *, #9529, .F. ) ;
#7539 = ADVANCED_FACE ( 'NONE', ( #3585 ), #4579, .F. ) ;
#7540 = CARTESIAN_POINT ( 'NONE',  ( 1.500000000000001332, 0.000000000000000000, 0.000000000000000000 ) ) ;
#7541 = ADVANCED_FACE ( 'NONE', ( #10954 ), #2392, .F. ) ;
#7542 = VERTEX_POINT ( 'NONE', #574 ) ;
#7543 = APPLICATION_PROTOCOL_DEFINITION ( 'draft international standard', 'automotive_design', 1998, #2171 ) ;
#7544 = EDGE_LOOP ( 'NONE', ( #6541, #1884, #1982, #9352 ) ) ;
#7545 = CYLINDRICAL_SURFACE ( 'NONE', #9020, 7.200000000007200640 ) ;
#7546 = CARTESIAN_POINT ( 'NONE',  ( 36.00000000000000711, -2.432816653220593039, 4.137801726981678030 ) ) ;
#7547 = EDGE_LOOP ( 'NONE', ( #11667, #8371, #11372, #445 ) ) ;
#7548 = ORIENTED_EDGE ( 'NONE', *, *, #9680, .F. ) ;
#7549 = DIRECTION ( 'NONE',  ( -1.000000000000000000, 0.000000000000000000, 0.000000000000000000 ) ) ;
#7550 = DIRECTION ( 'NONE',  ( -1.000000000000000000, 4.770489558936236458E-18, -6.855277276495154548E-34 ) ) ;
#7551 = DIRECTION ( 'NONE',  ( 1.000000000000000000, -0.000000000000000000, -0.000000000000000000 ) ) ;
#7552 = ORIENTED_EDGE ( 'NONE', *, *, #1731, .T. ) ;
#7553 = CARTESIAN_POINT ( 'NONE',  ( 4.999999999999999112, 0.000000000000000000, 0.000000000000000000 ) ) ;
#7554 = PRODUCT_DEFINITION ( 'UNKNOWN', '', #9649, #6027 ) ;
#7555 = VERTEX_POINT ( 'NONE', #3525 ) ;
#7556 = PRESENTATION_STYLE_ASSIGNMENT (( #10358 ) ) ;
#7557 = ORIENTED_EDGE ( 'NONE', *, *, #3799, .F. ) ;
#7558 = DIRECTION ( 'NONE',  ( -1.000000000000000000, -0.000000000000000000, -0.000000000000000000 ) ) ;
#7559 = ORIENTED_EDGE ( 'NONE', *, *, #9293, .T. ) ;
#7560 = DIRECTION ( 'NONE',  ( 1.000000000000000000, -4.770489558936235687E-18, 6.855277276495153692E-34 ) ) ;
#7561 = CARTESIAN_POINT ( 'NONE',  ( 4.999999999999999112, -19.60720892790260805, 11.14352537685167732 ) ) ;
#7562 = ADVANCED_FACE ( 'NONE', ( #7290 ), #2516, .T. ) ;
#7563 = EDGE_CURVE ( 'NONE', #4147, #3450, #6170, .T. ) ;
#7564 = CONICAL_SURFACE ( 'NONE', #9563, 3.790027207537782772, 0.08726646259971644615 ) ;
#7565 = CIRCLE ( 'NONE', #8167, 2.500000000000002220 ) ;
#7566 = AXIS2_PLACEMENT_3D ( 'NONE', #9668, #1091, #12270 ) ;
#7567 = CARTESIAN_POINT ( 'NONE',  ( 4.078421086530217288, -3.990950201428958621, -1.000000000000000000 ) ) ;
#7568 = CARTESIAN_POINT ( 'NONE',  ( 2.499999999999999556, -26.60936692326687592, -4.576198416197529539 ) ) ;
#7569 = ORIENTED_EDGE ( 'NONE', *, *, #8361, .T. ) ;
#7570 = VERTEX_POINT ( 'NONE', #11204 ) ;
#7571 = DIRECTION ( 'NONE',  ( 0.000000000000000000, 0.7900737791495477946, 0.6130117645692876316 ) ) ;
#7572 = CARTESIAN_POINT ( 'NONE',  ( 4.999999999999999112, 16.90755573046745397, 0.4834863907628708102 ) ) ;
#7573 = LINE ( 'NONE', #10313, #3690 ) ;
#7574 = ORIENTED_EDGE ( 'NONE', *, *, #6016, .T. ) ;
#7575 = DIRECTION ( 'NONE',  ( -1.000000000000000000, 0.000000000000000000, 0.000000000000000000 ) ) ;
#7576 = VECTOR ( 'NONE', #3342, 999.9999999999998863 ) ;
#7577 = AXIS2_PLACEMENT_3D ( 'NONE', #10615, #11533, #3741 ) ;
#7578 = DIRECTION ( 'NONE',  ( 0.000000000000000000, 0.000000000000000000, 1.000000000000000000 ) ) ;
#7579 = FACE_OUTER_BOUND ( 'NONE', #1362, .T. ) ;
#7580 = LINE ( 'NONE', #4009, #5040 ) ;
#7581 = DIRECTION ( 'NONE',  ( -2.731402571913187487E-17, -0.5883347247165658933, 0.8086174940555532764 ) ) ;
#7582 = AXIS2_PLACEMENT_3D ( 'NONE', #5578, #7719, #826 ) ;
#7583 = AXIS2_PLACEMENT_3D ( 'NONE', #5636, #5699, #2943 ) ;
#7584 = EDGE_LOOP ( 'NONE', ( #7292, #8128, #10911, #3078 ) ) ;
#7585 = CARTESIAN_POINT ( 'NONE',  ( 4.999999999999997335, 0.000000000000000000, 0.000000000000000000 ) ) ;
#7586 = CARTESIAN_POINT ( 'NONE',  ( 2.500000000000000000, 0.000000000000000000, 0.000000000000000000 ) ) ;
#7587 = AXIS2_PLACEMENT_3D ( 'NONE', #9055, #221, #5101 ) ;
#7588 = ORIENTED_EDGE ( 'NONE', *, *, #5846, .T. ) ;
#7589 = CARTESIAN_POINT ( 'NONE',  ( -1.500000000000001332, 7.041719095097280880E-16, 5.750000000000000000 ) ) ;
#7590 = ORIENTED_EDGE ( 'NONE', *, *, #1906, .T. ) ;
#7591 = AXIS2_PLACEMENT_3D ( 'NONE', #9921, #9114, #9056 ) ;
#7592 = EDGE_CURVE ( 'NONE', #5277, #9895, #12348, .T. ) ;
#7593 = CARTESIAN_POINT ( 'NONE',  ( 17.00000000000000000, 0.000000000000000000, 0.000000000000000000 ) ) ;
#7594 = FACE_OUTER_BOUND ( 'NONE', #8001, .T. ) ;
#7595 = CARTESIAN_POINT ( 'NONE',  ( 4.999999999999999112, -21.74405275335762155, 15.58472803277448726 ) ) ;
#7596 = CARTESIAN_POINT ( 'NONE',  ( -36.00000000000000711, 0.000000000000000000, 0.000000000000000000 ) ) ;
#7597 = DIRECTION ( 'NONE',  ( 0.000000000000000000, -0.4999999999999888978, -0.8660254037844450359 ) ) ;
#7598 = ORIENTED_EDGE ( 'NONE', *, *, #1317, .F. ) ;
#7599 = ORIENTED_EDGE ( 'NONE', *, *, #9150, .T. ) ;
#7600 = DIRECTION ( 'NONE',  ( 0.000000000000000000, 0.000000000000000000, 1.000000000000000000 ) ) ;
#7601 = COLOUR_RGB ( '',1.000000000000000000, 0.9490196078431372140, 0.9098039215686274384 ) ;
#7602 = ORIENTED_EDGE ( 'NONE', *, *, #11881, .T. ) ;
#7603 = CARTESIAN_POINT ( 'NONE',  ( 0.000000000000000000, 2.791921004064568113, -22.37914155802282323 ) ) ;
#7604 = APPLICATION_PROTOCOL_DEFINITION ( 'draft international standard', 'automotive_design', 1998, #5206 ) ;
#7605 = AXIS2_PLACEMENT_3D ( 'NONE', #8650, #1008, #2895 ) ;
#7606 = ORIENTED_EDGE ( 'NONE', *, *, #1519, .T. ) ;
#7607 = AXIS2_PLACEMENT_3D ( 'NONE', #9814, #3249, #5113 ) ;
#7608 = DIRECTION ( 'NONE',  ( -1.000000000000000000, 0.000000000000000000, 0.000000000000000000 ) ) ;
#7609 = EDGE_CURVE ( 'NONE', #2927, #8297, #4519, .T. ) ;
#7610 = DIRECTION ( 'NONE',  ( -1.000000000000000000, 0.000000000000000000, -0.000000000000000000 ) ) ;
#7611 = ADVANCED_FACE ( 'NONE', ( #8337 ), #6470, .T. ) ;
#7612 = ORIENTED_EDGE ( 'NONE', *, *, #5728, .T. ) ;
#7613 = EDGE_CURVE ( 'NONE', #9690, #7970, #519, .T. ) ;
#7614 = COLOUR_RGB ( '',0.8941176470588234615, 0.8941176470588234615, 0.8941176470588234615 ) ;
#7615 = EDGE_LOOP ( 'NONE', ( #7956, #7678, #4524, #8199 ) ) ;
#7616 = CARTESIAN_POINT ( 'NONE',  ( 36.00000000000000711, -3.606021680338235225, -38.83193945118931367 ) ) ;
#7617 = CARTESIAN_POINT ( 'NONE',  ( 51.00000000000000000, 3.500000000000001332, -38.49999999999998579 ) ) ;
#7618 = CIRCLE ( 'NONE', #9416, 9.600000000009599077 ) ;
#7619 = VECTOR ( 'NONE', #12225, 1000.000000000000000 ) ;
#7620 = DIRECTION ( 'NONE',  ( 0.000000000000000000, -0.8386705679454229401, -0.5446390350150287496 ) ) ;
#7621 = DIRECTION ( 'NONE',  ( 0.000000000000000000, 0.000000000000000000, 1.000000000000000000 ) ) ;
#7622 = ORIENTED_EDGE ( 'NONE', *, *, #9180, .F. ) ;
#7623 = DIRECTION ( 'NONE',  ( 1.000000000000000000, -0.000000000000000000, -0.000000000000000000 ) ) ;
#7624 = VERTEX_POINT ( 'NONE', #7221 ) ;
#7625 = EDGE_LOOP ( 'NONE', ( #5509, #6169, #7527, #3364, #10270, #4614, #4228, #11414 ) ) ;
#7626 = MECHANICAL_DESIGN_GEOMETRIC_PRESENTATION_REPRESENTATION (  '', ( #7661 ), #8220 ) ;
#7627 = VECTOR ( 'NONE', #3978, 1000.000000000000000 ) ;
#7628 = CARTESIAN_POINT ( 'NONE',  ( 0.000000000000000000, 6.799999999999999822, 1.500000000000000000 ) ) ;
#7629 = CIRCLE ( 'NONE', #6428, 0.2000000000000000944 ) ;
#7630 = AXIS2_PLACEMENT_3D ( 'NONE', #6673, #10470, #7860 ) ;
#7631 = EDGE_LOOP ( 'NONE', ( #7289, #3171, #10682, #11464, #7086, #6815 ) ) ;
#7632 = CARTESIAN_POINT ( 'NONE',  ( 42.00000000000000000, 1.908195823574506293E-17, -41.99999999999998579 ) ) ;
#7633 = EDGE_CURVE ( 'NONE', #2426, #6734, #11024, .T. ) ;
#7634 = ADVANCED_FACE ( 'NONE', ( #1762 ), #12258, .T. ) ;
#7635 = DIRECTION ( 'NONE',  ( 1.000000000000000000, -0.000000000000000000, -0.000000000000000000 ) ) ;
#7636 = AXIS2_PLACEMENT_3D ( 'NONE', #12138, #7352, #7414 ) ;
#7637 = CIRCLE ( 'NONE', #4428, 27.00000000002699707 ) ;
#7638 = AXIS2_PLACEMENT_3D ( 'NONE', #10159, #12273, #11040 ) ;
#7639 = CIRCLE ( 'NONE', #41, 9.600000000009600853 ) ;
#7640 = CARTESIAN_POINT ( 'NONE',  ( 0.000000000000000000, -26.60936692326693631, 4.576198416197160057 ) ) ;
#7641 = LINE ( 'NONE', #5626, #9450 ) ;
#7642 = VERTEX_POINT ( 'NONE', #9400 ) ;
#7643 = CARTESIAN_POINT ( 'NONE',  ( -1.500000000000001332, 9.123618653647779187E-16, 7.399999999999999467 ) ) ;
#7644 = APPLICATION_PROTOCOL_DEFINITION ( 'draft international standard', 'automotive_design', 1998, #3872 ) ;
#7645 = DIRECTION ( 'NONE',  ( 0.000000000000000000, -0.4999999999999888423, -0.8660254037844451469 ) ) ;
#7646 = DIRECTION ( 'NONE',  ( 0.000000000000000000, -0.5000000000000012212, -0.8660254037844380415 ) ) ;
#7647 = EDGE_CURVE ( 'NONE', #11273, #4720, #83, .T. ) ;
#7648 = EDGE_LOOP ( 'NONE', ( #963, #9503 ) ) ;
#7649 = CARTESIAN_POINT ( 'NONE',  ( 4.999999999999999112, -1.561154383803080581, -20.18872947935932771 ) ) ;
#7650 = ADVANCED_FACE ( 'NONE', ( #6524 ), #3899, .F. ) ;
#7651 =( GEOMETRIC_REPRESENTATION_CONTEXT ( 3 ) GLOBAL_UNCERTAINTY_ASSIGNED_CONTEXT ( ( #4899 ) ) GLOBAL_UNIT_ASSIGNED_CONTEXT ( ( #1293, #1113, #11535 ) ) REPRESENTATION_CONTEXT ( 'NONE', 'WORKASPACE' ) );
#7652 = CIRCLE ( 'NONE', #9846, 2.149999999999999023 ) ;
#7653 = CIRCLE ( 'NONE', #3441, 6.080745460913608902 ) ;
#7654 = AXIS2_PLACEMENT_3D ( 'NONE', #5706, #6843, #8522 ) ;
#7655 = DIRECTION ( 'NONE',  ( -0.000000000000000000, -0.000000000000000000, 1.000000000000000000 ) ) ;
#7656 = LINE ( 'NONE', #11446, #4007 ) ;
#7657 = CIRCLE ( 'NONE', #5174, 0.7499999999999997780 ) ;
#7658 = CYLINDRICAL_SURFACE ( 'NONE', #8653, 5.525000000000000355 ) ;
#7659 = DIRECTION ( 'NONE',  ( 0.000000000000000000, 0.000000000000000000, -1.000000000000000000 ) ) ;
#7660 = CIRCLE ( 'NONE', #9255, 4.800000000000000711 ) ;
#7661 = STYLED_ITEM ( 'NONE', ( #3852 ), #10918 ) ;
#7662 = VERTEX_POINT ( 'NONE', #11384 ) ;
#7663 = DIRECTION ( 'NONE',  ( 1.000000000000000000, 0.000000000000000000, 0.000000000000000000 ) ) ;
#7664 = VECTOR ( 'NONE', #3375, 1000.000000000000000 ) ;
#7665 = CARTESIAN_POINT ( 'NONE',  ( 0.000000000000000000, 5.955107813822862362, -26.33508479058314933 ) ) ;
#7666 = ORIENTED_EDGE ( 'NONE', *, *, #7829, .T. ) ;
#7667 = CARTESIAN_POINT ( 'NONE',  ( 17.00000000000000000, 0.000000000000000000, 0.000000000000000000 ) ) ;
#7668 = ORIENTED_EDGE ( 'NONE', *, *, #10597, .F. ) ;
#7669 = CIRCLE ( 'NONE', #3265, 9.600000000009604406 ) ;
#7670 =( NAMED_UNIT ( * ) PLANE_ANGLE_UNIT ( ) SI_UNIT ( $, .RADIAN. ) );
#7671 = DIRECTION ( 'NONE',  ( 0.000000000000000000, -0.7071067811865537900, 0.7071067811865414665 ) ) ;
#7672 = DIRECTION ( 'NONE',  ( 0.000000000000000000, 0.000000000000000000, 1.000000000000000000 ) ) ;
#7673 = LINE ( 'NONE', #7728, #2046 ) ;
#7674 = LINE ( 'NONE', #1093, #3434 ) ;
#7675 = ORIENTED_EDGE ( 'NONE', *, *, #9074, .F. ) ;
#7676 = ORIENTED_EDGE ( 'NONE', *, *, #10982, .F. ) ;
#7677 = DIRECTION ( 'NONE',  ( 0.000000000000000000, 0.6828850436591806794, 0.7305258497456466049 ) ) ;
#7678 = ORIENTED_EDGE ( 'NONE', *, *, #5728, .F. ) ;
#7679 = DIRECTION ( 'NONE',  ( 0.000000000000000000, 0.000000000000000000, -1.000000000000000000 ) ) ;
#7680 = ITEM_DEFINED_TRANSFORMATION ( 'NONE', 'NONE', #4050,  #6056 ) ;
#7681 = ORIENTED_EDGE ( 'NONE', *, *, #8917, .T. ) ;
#7682 = EDGE_LOOP ( 'NONE', ( #1813, #2394, #4801, #3891 ) ) ;
#7683 = ORIENTED_EDGE ( 'NONE', *, *, #11514, .T. ) ;
#7684 = CARTESIAN_POINT ( 'NONE',  ( 4.999999999999999112, -2.791921004064401579, 22.37914155802284100 ) ) ;
#7685 = CARTESIAN_POINT ( 'NONE',  ( 0.000000000000000000, -20.18872947935932061, 1.561154383803151191 ) ) ;
#7686 = AXIS2_PLACEMENT_3D ( 'NONE', #11891, #11839, #7104 ) ;
#7687 = DIRECTION ( 'NONE',  ( -1.000000000000000000, -0.000000000000000000, 0.000000000000000000 ) ) ;
#7688 = CARTESIAN_POINT ( 'NONE',  ( -20.00000000000000000, 0.000000000000000000, 0.000000000000000000 ) ) ;
#7689 = EDGE_CURVE ( 'NONE', #8093, #10792, #1384, .T. ) ;
#7690 = ORIENTED_EDGE ( 'NONE', *, *, #4713, .T. ) ;
#7691 = LINE ( 'NONE', #5610, #2172 ) ;
#7692 = VERTEX_POINT ( 'NONE', #6722 ) ;
#7693 = EDGE_CURVE ( 'NONE', #10319, #2452, #3982, .T. ) ;
#7694 = EDGE_LOOP ( 'NONE', ( #2760, #10536 ) ) ;
#7695 = CARTESIAN_POINT ( 'NONE',  ( 43.00000000000000000, -3.058102613202345665, 3.699730856038719207 ) ) ;
#7696 = AXIS2_PLACEMENT_3D ( 'NONE', #1960, #6665, #8528 ) ;
#7697 = ORIENTED_EDGE ( 'NONE', *, *, #10444, .T. ) ;
#7698 = CARTESIAN_POINT ( 'NONE',  ( 33.00000000000000000, 0.000000000000000000, -7.500000000000000888 ) ) ;
#7699 = LINE ( 'NONE', #8814, #3606 ) ;
#7700 = ADVANCED_FACE ( 'NONE', ( #5650 ), #2704, .T. ) ;
#7701 = AXIS2_PLACEMENT_3D ( 'NONE', #8146, #6384, #5456 ) ;
#7702 = DIRECTION ( 'NONE',  ( 0.000000000000000000, 0.000000000000000000, -1.000000000000000000 ) ) ;
#7703 = LINE ( 'NONE', #11491, #5446 ) ;
#7704 = VERTEX_POINT ( 'NONE', #1833 ) ;
#7705 = DIRECTION ( 'NONE',  ( -1.000000000000000000, 0.000000000000000000, 0.000000000000000000 ) ) ;
#7706 = EDGE_CURVE ( 'NONE', #9748, #2794, #7781, .T. ) ;
#7707 =( NAMED_UNIT ( * ) PLANE_ANGLE_UNIT ( ) SI_UNIT ( $, .RADIAN. ) );
#7708 = CARTESIAN_POINT ( 'NONE',  ( -15.00000000000000000, 30.00000000000000711, 2.000000000000000000 ) ) ;
#7709 = EDGE_CURVE ( 'NONE', #1163, #11209, #7389, .T. ) ;
#7710 = EDGE_CURVE ( 'NONE', #9875, #5720, #10769, .T. ) ;
#7711 = DIRECTION ( 'NONE',  ( 0.000000000000000000, 0.000000000000000000, -1.000000000000000000 ) ) ;
#7712 = ORIENTED_EDGE ( 'NONE', *, *, #9136, .F. ) ;
#7713 = FACE_OUTER_BOUND ( 'NONE', #1355, .T. ) ;
#7714 = CARTESIAN_POINT ( 'NONE',  ( 0.000000000000000000, 0.000000000000000000, -1.000000000000000000 ) ) ;
#7715 = EDGE_CURVE ( 'NONE', #7170, #2396, #991, .T. ) ;
#7716 = FACE_OUTER_BOUND ( 'NONE', #7932, .T. ) ;
#7717 = DIRECTION ( 'NONE',  ( 1.000000000000000000, 0.000000000000000000, 0.000000000000000000 ) ) ;
#7718 = ORIENTED_EDGE ( 'NONE', *, *, #7633, .T. ) ;
#7719 = DIRECTION ( 'NONE',  ( -1.000000000000000000, 0.000000000000000000, 0.000000000000000000 ) ) ;
#7720 = DIRECTION ( 'NONE',  ( 1.000000000000000000, -4.770489558936235687E-18, 6.855277276495153692E-34 ) ) ;
#7721 = VERTEX_POINT ( 'NONE', #9523 ) ;
#7722 = CARTESIAN_POINT ( 'NONE',  ( 4.999999999999999112, 0.000000000000000000, 0.000000000000000000 ) ) ;
#7723 = EDGE_LOOP ( 'NONE', ( #10624, #3817, #2153 ) ) ;
#7724 = CYLINDRICAL_SURFACE ( 'NONE', #3809, 2.000000000000000000 ) ;
#7725 = CARTESIAN_POINT ( 'NONE',  ( 15.00000000000000355, 40.00000000000000711, -1.999999999999998224 ) ) ;
#7726 = ADVANCED_FACE ( 'NONE', ( #6771 ), #5837, .T. ) ;
#7727 = EDGE_CURVE ( 'NONE', #4119, #718, #3590, .T. ) ;
#7728 = CARTESIAN_POINT ( 'NONE',  ( 46.00000000000000000, 1.456773409934505593E-31, -36.99999999999998579 ) ) ;
#7729 = FACE_OUTER_BOUND ( 'NONE', #6536, .T. ) ;
#7730 = PRODUCT ( 'slotted pan head screw_iso_ISO 1580 - M4 x 12 - 12N', 'slotted pan head screw_iso_ISO 1580 - M4 x 12 - 12N', '', ( #2854 ) ) ;
#7731 = ORIENTED_EDGE ( 'NONE', *, *, #662, .T. ) ;
#7732 = ORIENTED_EDGE ( 'NONE', *, *, #8383, .F. ) ;
#7733 = VERTEX_POINT ( 'NONE', #10389 ) ;
#7734 = FACE_BOUND ( 'NONE', #2331, .T. ) ;
#7735 = SHAPE_DEFINITION_REPRESENTATION ( #10818, #8907 ) ;
#7736 = ORIENTED_EDGE ( 'NONE', *, *, #7843, .T. ) ;
#7737 = ORIENTED_EDGE ( 'NONE', *, *, #8255, .F. ) ;
#7738 = ORIENTED_EDGE ( 'NONE', *, *, #9556, .F. ) ;
#7739 = LINE ( 'NONE', #4792, #5181 ) ;
#7740 = DIRECTION ( 'NONE',  ( 0.000000000000000000, 0.000000000000000000, 1.000000000000000000 ) ) ;
#7741 = CARTESIAN_POINT ( 'NONE',  ( 4.999999999999999112, 8.527191590521072229, 11.41582255376076027 ) ) ;
#7742 = DIRECTION ( 'NONE',  ( 0.000000000000000000, 0.8660254037844398178, -0.4999999999999980571 ) ) ;
#7743 = ORIENTED_EDGE ( 'NONE', *, *, #11947, .F. ) ;
#7744 = CARTESIAN_POINT ( 'NONE',  ( 4.999999999999999112, -19.60720892790245529, -11.14352537685195266 ) ) ;
#7745 = ORIENTED_EDGE ( 'NONE', *, *, #8938, .F. ) ;
#7746 = ORIENTED_EDGE ( 'NONE', *, *, #305, .T. ) ;
#7747 = CARTESIAN_POINT ( 'NONE',  ( -26.00000000000000355, 30.00000000000000711, -19.99999999999998934 ) ) ;
#7748 = ORIENTED_EDGE ( 'NONE', *, *, #11783, .T. ) ;
#7749 = CARTESIAN_POINT ( 'NONE',  ( 51.00000000000000000, -3.499999999999998668, -38.49999999999998579 ) ) ;
#7750 = EDGE_CURVE ( 'NONE', #2996, #1270, #7985, .T. ) ;
#7751 = DIRECTION ( 'NONE',  ( -1.000000000000000000, -0.000000000000000000, -0.000000000000000000 ) ) ;
#7752 = ADVANCED_FACE ( 'NONE', ( #3653 ), #8, .T. ) ;
#7753 = ORIENTED_EDGE ( 'NONE', *, *, #10054, .T. ) ;
#7754 = FACE_OUTER_BOUND ( 'NONE', #5242, .T. ) ;
#7755 = CARTESIAN_POINT ( 'NONE',  ( 5.000000000000000000, 6.799999999999999822, 0.000000000000000000 ) ) ;
#7756 = VERTEX_POINT ( 'NONE', #5708 ) ;
#7757 = PRODUCT_CONTEXT ( 'NONE', #3308, 'mechanical' ) ;
#7758 = DIRECTION ( 'NONE',  ( 0.000000000000000000, 0.7900737791495477946, 0.6130117645692876316 ) ) ;
#7759 = FACE_BOUND ( 'NONE', #5198, .T. ) ;
#7760 = ORIENTED_EDGE ( 'NONE', *, *, #11893, .T. ) ;
#7761 = LINE ( 'NONE', #10378, #11166 ) ;
#7762 = EDGE_CURVE ( 'NONE', #542, #1039, #6983, .T. ) ;
#7763 = EDGE_CURVE ( 'NONE', #1039, #6055, #11450, .T. ) ;
#7764 = AXIS2_PLACEMENT_3D ( 'NONE', #7097, #4201, #8912 ) ;
#7765 = ADVANCED_FACE ( 'NONE', ( #8841, #1374 ), #11639, .F. ) ;
#7766 = DIRECTION ( 'NONE',  ( -1.000000000000000000, -0.000000000000000000, -0.000000000000000000 ) ) ;
#7767 = FACE_OUTER_BOUND ( 'NONE', #2535, .T. ) ;
#7768 = DIRECTION ( 'NONE',  ( 1.000000000000000000, -0.000000000000000000, -0.000000000000000000 ) ) ;
#7769 = DIRECTION ( 'NONE',  ( -1.472782982004545120E-17, -0.8086174940555532764, -0.5883347247165658933 ) ) ;
#7770 = ORIENTED_EDGE ( 'NONE', *, *, #6547, .F. ) ;
#7771 = DIRECTION ( 'NONE',  ( 0.000000000000000000, 0.000000000000000000, 1.000000000000000000 ) ) ;
#7772 = FACE_OUTER_BOUND ( 'NONE', #9125, .T. ) ;
#7773 = CIRCLE ( 'NONE', #2170, 14.24900000001425049 ) ;
#7774 = VERTEX_POINT ( 'NONE', #266 ) ;
#7775 = CARTESIAN_POINT ( 'NONE',  ( -25.00000000000000000, 0.000000000000000000, 0.000000000000000000 ) ) ;
#7776 =( REPRESENTATION_RELATIONSHIP ('NONE','NONE', #9709, #5877 ) REPRESENTATION_RELATIONSHIP_WITH_TRANSFORMATION ( #7294 )SHAPE_REPRESENTATION_RELATIONSHIP( ) );
#7777 = UNCERTAINTY_MEASURE_WITH_UNIT (LENGTH_MEASURE( 1.000000000000000082E-05 ), #2594, 'distance_accuracy_value', 'NONE');
#7778 = AXIS2_PLACEMENT_3D ( 'NONE', #2069, #6563, #1122 ) ;
#7779 = ORIENTED_EDGE ( 'NONE', *, *, #10305, .T. ) ;
#7780 = PRODUCT_DEFINITION ( 'UNKNOWN', '', #11226, #3152 ) ;
#7781 = CIRCLE ( 'NONE', #5983, 14.24900000001425227 ) ;
#7782 = CARTESIAN_POINT ( 'NONE',  ( 4.999999999999999112, 11.14352537685202016, -19.60720892790241265 ) ) ;
#7783 = CARTESIAN_POINT ( 'NONE',  ( 46.00000000000000000, 1.444447458290426890E-31, -41.99999999999998579 ) ) ;
#7784 = VECTOR ( 'NONE', #1610, 1000.000000000000000 ) ;
#7785 = CIRCLE ( 'NONE', #6586, 2.041999999999999815 ) ;
#7786 = DIRECTION ( 'NONE',  ( 0.000000000000000000, 0.000000000000000000, -1.000000000000000000 ) ) ;
#7787 = CARTESIAN_POINT ( 'NONE',  ( 5.000000000000000000, 0.000000000000000000, 0.000000000000000000 ) ) ;
#7788 = ORIENTED_EDGE ( 'NONE', *, *, #10152, .F. ) ;
#7789 = CYLINDRICAL_SURFACE ( 'NONE', #5053, 21.00000000002100009 ) ;
#7790 = EDGE_LOOP ( 'NONE', ( #6685, #2057, #5932, #3792 ) ) ;
#7791 = LINE ( 'NONE', #5918, #12243 ) ;
#7792 = UNCERTAINTY_MEASURE_WITH_UNIT (LENGTH_MEASURE( 1.000000000000000082E-05 ), #10329, 'distance_accuracy_value', 'NONE');
#7793 = VERTEX_POINT ( 'NONE', #10886 ) ;
#7794 = AXIS2_PLACEMENT_3D ( 'NONE', #8680, #10673, #10855 ) ;
#7795 = CIRCLE ( 'NONE', #11141, 4.000000000000003553 ) ;
#7796 = EDGE_CURVE ( 'NONE', #6970, #9064, #2316, .T. ) ;
#7797 = EDGE_CURVE ( 'NONE', #11913, #661, #9377, .T. ) ;
#7798 = VERTEX_POINT ( 'NONE', #3953 ) ;
#7799 = ORIENTED_EDGE ( 'NONE', *, *, #6390, .F. ) ;
#7800 = DIRECTION ( 'NONE',  ( -1.000000000000000000, -0.000000000000000000, -0.000000000000000000 ) ) ;
#7801 = CYLINDRICAL_SURFACE ( 'NONE', #1021, 6.080745460913608902 ) ;
#7802 = CARTESIAN_POINT ( 'NONE',  ( 4.999999999999999112, -11.41582255376079047, 8.527191590521034925 ) ) ;
#7803 = DIRECTION ( 'NONE',  ( 0.000000000000000000, -6.866613759067995433E-15, 1.000000000000000000 ) ) ;
#7804 = AXIS2_PLACEMENT_3D ( 'NONE', #6034, #2143, #11828 ) ;
#7805 = VERTEX_POINT ( 'NONE', #11694 ) ;
#7806 = VECTOR ( 'NONE', #2351, 1000.000000000000000 ) ;
#7807 = DIRECTION ( 'NONE',  ( 0.000000000000000000, 0.000000000000000000, 1.000000000000000000 ) ) ;
#7808 = VERTEX_POINT ( 'NONE', #3092 ) ;
#7809 = ORIENTED_EDGE ( 'NONE', *, *, #5661, .T. ) ;
#7810 = DIRECTION ( 'NONE',  ( 0.000000000000000000, 1.000000000000000000, 0.000000000000000000 ) ) ;
#7811 = ORIENTED_EDGE ( 'NONE', *, *, #9979, .T. ) ;
#7812 = CARTESIAN_POINT ( 'NONE',  ( 42.00000000000000000, -5.000000000000004441, -41.99999999999998579 ) ) ;
#7813 =( GEOMETRIC_REPRESENTATION_CONTEXT ( 3 ) GLOBAL_UNCERTAINTY_ASSIGNED_CONTEXT ( ( #12 ) ) GLOBAL_UNIT_ASSIGNED_CONTEXT ( ( #6900, #8836, #7080 ) ) REPRESENTATION_CONTEXT ( 'NONE', 'WORKASPACE' ) );
#7814 = VECTOR ( 'NONE', #2106, 1000.000000000000000 ) ;
#7815 = DIRECTION ( 'NONE',  ( -0.5000000000000051070, 0.000000000000000000, 0.8660254037844355990 ) ) ;
#7816 = ORIENTED_EDGE ( 'NONE', *, *, #5787, .F. ) ;
#7817 = DIRECTION ( 'NONE',  ( -1.000000000000000000, 0.000000000000000000, 0.000000000000000000 ) ) ;
#7818 = DIRECTION ( 'NONE',  ( -1.000000000000000000, 0.000000000000000000, -0.000000000000000000 ) ) ;
#7819 = VECTOR ( 'NONE', #11598, 1000.000000000000000 ) ;
#7820 = ORIENTED_EDGE ( 'NONE', *, *, #10262, .F. ) ;
#7821 = VECTOR ( 'NONE', #8109, 1000.000000000000000 ) ;
#7822 = FACE_OUTER_BOUND ( 'NONE', #6523, .T. ) ;
#7823 = SHAPE_REPRESENTATION_RELATIONSHIP ( 'NONE' , 'NONE' ,  #7946, #11675 ) ;
#7824 = VECTOR ( 'NONE', #1868, 1000.000000000000000 ) ;
#7825 = CARTESIAN_POINT ( 'NONE',  ( 1.199999999999999956, 3.294826241329278276E-16, -2.690429798716874377 ) ) ;
#7826 = VECTOR ( 'NONE', #7532, 1000.000000000000000 ) ;
#7827 = AXIS2_PLACEMENT_3D ( 'NONE', #4481, #10915, #8248 ) ;
#7828 = CARTESIAN_POINT ( 'NONE',  ( 1.600000000000000089, 0.000000000000000000, 7.000000000000000000 ) ) ;
#7829 = EDGE_CURVE ( 'NONE', #6360, #11478, #8026, .T. ) ;
#7830 = ORIENTED_EDGE ( 'NONE', *, *, #7034, .T. ) ;
#7831 = DIRECTION ( 'NONE',  ( -1.000000000000000000, -0.000000000000000000, -0.000000000000000000 ) ) ;
#7832 = MECHANICAL_DESIGN_GEOMETRIC_PRESENTATION_REPRESENTATION (  '', ( #4821 ), #7428 ) ;
#7833 = AXIS2_PLACEMENT_3D ( 'NONE', #7196, #1867, #5606 ) ;
#7834 = VECTOR ( 'NONE', #10019, 1000.000000000000000 ) ;
#7835 = PRODUCT_DEFINITION_SHAPE ( 'NONE', 'NONE',  #12355 ) ;
#7836 = VECTOR ( 'NONE', #11887, 1000.000000000000000 ) ;
#7837 = VECTOR ( 'NONE', #5199, 1000.000000000000000 ) ;
#7838 = CARTESIAN_POINT ( 'NONE',  ( 24.00000000000000000, 7.347880794884119736E-16, -35.99999999999999289 ) ) ;
#7839 = CARTESIAN_POINT ( 'NONE',  ( 26.00000000000000355, -12.50000000000000000, -24.50000000000000000 ) ) ;
#7840 = CARTESIAN_POINT ( 'NONE',  ( -38.00000000000000000, 0.000000000000000000, -5.999999999999999112 ) ) ;
#7841 = CARTESIAN_POINT ( 'NONE',  ( 0.000000000000000000, 15.22291137398921990, 14.46592441914969918 ) ) ;
#7842 = ORIENTED_EDGE ( 'NONE', *, *, #1112, .F. ) ;
#7843 = EDGE_CURVE ( 'NONE', #3524, #6028, #4135, .T. ) ;
#7844 = DIRECTION ( 'NONE',  ( 0.000000000000000000, 1.000000000000000000, 3.373073425507084106E-15 ) ) ;
#7845 = FACE_OUTER_BOUND ( 'NONE', #1874, .T. ) ;
#7846 = STYLED_ITEM ( 'NONE', ( #7556 ), #4814 ) ;
#7847 = AXIS2_PLACEMENT_3D ( 'NONE', #8789, #957, #7786 ) ;
#7848 = EDGE_LOOP ( 'NONE', ( #9027, #7100, #5327, #423 ) ) ;
#7849 = CYLINDRICAL_SURFACE ( 'NONE', #6289, 2.500000000000002220 ) ;
#7850 = AXIS2_PLACEMENT_3D ( 'NONE', #12034, #10161, #2529 ) ;
#7851 = EDGE_CURVE ( 'NONE', #9474, #11456, #9781, .T. ) ;
#7852 = ORIENTED_EDGE ( 'NONE', *, *, #3332, .F. ) ;
#7853 = CARTESIAN_POINT ( 'NONE',  ( -10.00000000000000000, 0.000000000000000000, 0.000000000000000000 ) ) ;
#7854 = AXIS2_PLACEMENT_3D ( 'NONE', #2949, #12310, #8581 ) ;
#7855 = CIRCLE ( 'NONE', #8445, 5.000000000000000000 ) ;
#7856 = LINE ( 'NONE', #902, #1204 ) ;
#7857 = DIRECTION ( 'NONE',  ( 0.000000000000000000, 0.7071067811865439090, 0.7071067811865512365 ) ) ;
#7858 = AXIS2_PLACEMENT_3D ( 'NONE', #9089, #501, #5321 ) ;
#7859 = DIRECTION ( 'NONE',  ( 0.000000000000000000, 0.000000000000000000, 1.000000000000000000 ) ) ;
#7860 = DIRECTION ( 'NONE',  ( 0.000000000000000000, 0.000000000000000000, 1.000000000000000000 ) ) ;
#7861 = ORIENTED_EDGE ( 'NONE', *, *, #2493, .T. ) ;
#7862 = DIRECTION ( 'NONE',  ( 0.000000000000000000, 0.000000000000000000, 1.000000000000000000 ) ) ;
#7863 = ORIENTED_EDGE ( 'NONE', *, *, #7988, .T. ) ;
#7864 = LINE ( 'NONE', #11657, #11457 ) ;
#7865 = EDGE_CURVE ( 'NONE', #7160, #9505, #9581, .T. ) ;
#7866 = APPLICATION_PROTOCOL_DEFINITION ( 'draft international standard', 'automotive_design', 1998, #4100 ) ;
#7867 = ADVANCED_FACE ( 'NONE', ( #5955 ), #10759, .T. ) ;
#7868 = ORIENTED_EDGE ( 'NONE', *, *, #11266, .F. ) ;
#7869 = ADVANCED_FACE ( 'NONE', ( #10831 ), #11563, .T. ) ;
#7870 = AXIS2_PLACEMENT_3D ( 'NONE', #625, #1630, #4445 ) ;
#7871 = CARTESIAN_POINT ( 'NONE',  ( 0.000000000000000000, 21.74405275335758247, 5.984728032765037398 ) ) ;
#7872 = VERTEX_POINT ( 'NONE', #1197 ) ;
#7873 = FACE_OUTER_BOUND ( 'NONE', #5548, .T. ) ;
#7874 = CARTESIAN_POINT ( 'NONE',  ( 4.999999999999999112, 16.90755573046746107, -0.4834863907626340551 ) ) ;
#7875 = CARTESIAN_POINT ( 'NONE',  ( 26.00000000000000355, 0.000000000000000000, 20.00000000000001066 ) ) ;
#7876 = CARTESIAN_POINT ( 'NONE',  ( 4.999999999999999112, -4.576198416197066798, -26.60936692326695407 ) ) ;
#7877 = ORIENTED_EDGE ( 'NONE', *, *, #3877, .F. ) ;
#7878 = EDGE_CURVE ( 'NONE', #681, #6632, #5790, .T. ) ;
#7879 = ORIENTED_EDGE ( 'NONE', *, *, #1879, .F. ) ;
#7880 = EDGE_LOOP ( 'NONE', ( #11109, #3225 ) ) ;
#7881 = LINE ( 'NONE', #3177, #4419 ) ;
#7882 = ORIENTED_EDGE ( 'NONE', *, *, #9136, .T. ) ;
#7883 = DIRECTION ( 'NONE',  ( 0.000000000000000000, -6.987080667121815555E-15, 1.000000000000000000 ) ) ;
#7884 = AXIS2_PLACEMENT_3D ( 'NONE', #7972, #10041, #5286 ) ;
#7885 = LINE ( 'NONE', #2064, #6607 ) ;
#7886 = ORIENTED_EDGE ( 'NONE', *, *, #6498, .T. ) ;
#7887 = EDGE_CURVE ( 'NONE', #10787, #9456, #2374, .T. ) ;
#7888 = DIRECTION ( 'NONE',  ( -1.000000000000000000, 0.000000000000000000, 0.000000000000000000 ) ) ;
#7889 = DIRECTION ( 'NONE',  ( 0.000000000000000000, 0.000000000000000000, -1.000000000000000000 ) ) ;
#7890 = VERTEX_POINT ( 'NONE', #6846 ) ;
#7891 = CARTESIAN_POINT ( 'NONE',  ( 0.000000000000000000, 0.000000000000000000, -1.000000000000000000 ) ) ;
#7892 = AXIS2_PLACEMENT_3D ( 'NONE', #11946, #1654, #10149 ) ;
#7893 = DIRECTION ( 'NONE',  ( -1.000000000000000000, 0.000000000000000000, -0.000000000000000000 ) ) ;
#7894 = CARTESIAN_POINT ( 'NONE',  ( 36.00000000000000711, 0.000000000000000000, 0.000000000000000000 ) ) ;
#7895 = ORIENTED_EDGE ( 'NONE', *, *, #6609, .F. ) ;
#7896 = CARTESIAN_POINT ( 'NONE',  ( 25.00000000000000000, 3.061616997868383043E-15, 25.00000000000000000 ) ) ;
#7897 = AXIS2_PLACEMENT_3D ( 'NONE', #11371, #2815, #11441 ) ;
#7898 = DIRECTION ( 'NONE',  ( -1.000000000000000000, 0.000000000000000000, 0.000000000000000000 ) ) ;
#7899 = DIRECTION ( 'NONE',  ( 0.000000000000000000, 0.000000000000000000, 1.000000000000000000 ) ) ;
#7900 = FACE_OUTER_BOUND ( 'NONE', #11642, .T. ) ;
#7901 = DIRECTION ( 'NONE',  ( 0.000000000000000000, -0.000000000000000000, 1.000000000000000000 ) ) ;
#7902 = VERTEX_POINT ( 'NONE', #9898 ) ;
#7903 = CARTESIAN_POINT ( 'NONE',  ( 70.79898987322334847, 3.500000000000001332, -38.49999999999998579 ) ) ;
#7904 = DIRECTION ( 'NONE',  ( 0.000000000000000000, 0.000000000000000000, 1.000000000000000000 ) ) ;
#7905 = ORIENTED_EDGE ( 'NONE', *, *, #9903, .F. ) ;
#7906 = CARTESIAN_POINT ( 'NONE',  ( 2.399999999999999467, 2.000000000000000000, 0.000000000000000000 ) ) ;
#7907 = AXIS2_PLACEMENT_3D ( 'NONE', #3004, #7945, #3436 ) ;
#7908 = ORIENTED_EDGE ( 'NONE', *, *, #6921, .T. ) ;
#7909 = CARTESIAN_POINT ( 'NONE',  ( 51.00000000000000000, 0.000000000000000000, -41.99999999999999289 ) ) ;
#7910 = EDGE_CURVE ( 'NONE', #3410, #9763, #10651, .T. ) ;
#7911 = CYLINDRICAL_SURFACE ( 'NONE', #1405, 27.00000000002699707 ) ;
#7912 = CARTESIAN_POINT ( 'NONE',  ( 4.999999999999999112, 16.90755573046746107, 6.716513609244568528 ) ) ;
#7913 = EDGE_CURVE ( 'NONE', #8750, #9528, #3380, .T. ) ;
#7914 = DIRECTION ( 'NONE',  ( -1.000000000000000000, -0.000000000000000000, 0.000000000000000000 ) ) ;
#7915 = DIRECTION ( 'NONE',  ( 0.000000000000000000, -1.000000000000000000, -1.036015409262890124E-14 ) ) ;
#7916 = ORIENTED_EDGE ( 'NONE', *, *, #1634, .F. ) ;
#7917 =( LENGTH_UNIT ( ) NAMED_UNIT ( * ) SI_UNIT ( .MILLI., .METRE. ) );
#7918 = VERTEX_POINT ( 'NONE', #4949 ) ;
#7919 = FACE_OUTER_BOUND ( 'NONE', #9077, .T. ) ;
#7920 = ITEM_DEFINED_TRANSFORMATION ( 'NONE', 'NONE', #3857,  #6056 ) ;
#7921 = EDGE_LOOP ( 'NONE', ( #5036, #6312, #7245, #12097 ) ) ;
#7922 = ADVANCED_FACE ( 'NONE', ( #11747 ), #3206, .T. ) ;
#7923 = CARTESIAN_POINT ( 'NONE',  ( 4.999999999999999112, 0.000000000000000000, 0.000000000000000000 ) ) ;
#7924 = VERTEX_POINT ( 'NONE', #7020 ) ;
#7925 = DIRECTION ( 'NONE',  ( 0.000000000000000000, 0.000000000000000000, 1.000000000000000000 ) ) ;
#7926 = DIRECTION ( 'NONE',  ( -1.000000000000000000, 0.000000000000000000, 0.000000000000000000 ) ) ;
#7927 = EDGE_CURVE ( 'NONE', #9505, #11408, #1318, .T. ) ;
#7928 = DIRECTION ( 'NONE',  ( 0.000000000000000000, 0.000000000000000000, -1.000000000000000000 ) ) ;
#7930 = EDGE_CURVE ( 'NONE', #9620, #1234, #7739, .T. ) ;
#7929 = CARTESIAN_POINT ( 'NONE',  ( 36.00000000000000711, 0.000000000000000000, -41.99999999999999289 ) ) ;
#7931 = ORIENTED_EDGE ( 'NONE', *, *, #3317, .F. ) ;
#7932 = EDGE_LOOP ( 'NONE', ( #667, #1036, #4139, #9865 ) ) ;
#7933 = ORIENTED_EDGE ( 'NONE', *, *, #2944, .F. ) ;
#7934 = FACE_OUTER_BOUND ( 'NONE', #6399, .T. ) ;
#7935 = DIRECTION ( 'NONE',  ( 0.000000000000000000, -0.9238795325112906243, 0.3826834323650805114 ) ) ;
#7936 = CARTESIAN_POINT ( 'NONE',  ( 33.00000000000000000, 0.000000000000000000, 0.000000000000000000 ) ) ;
#7937 = PRODUCT_DEFINITION ( 'UNKNOWN', '', #5847, #9029 ) ;
#7938 = APPLICATION_CONTEXT ( 'automotive_design' ) ;
#7939 = EDGE_LOOP ( 'NONE', ( #8437, #6746, #6086, #6619 ) ) ;
#7940 = DIRECTION ( 'NONE',  ( 0.000000000000000000, -6.987080667121817133E-15, 1.000000000000000000 ) ) ;
#7941 = CARTESIAN_POINT ( 'NONE',  ( -1.250000000000000000, -6.429618962271402616, -1.000000000000000000 ) ) ;
#7942 = ORIENTED_EDGE ( 'NONE', *, *, #3568, .T. ) ;
#7943 = DIRECTION ( 'NONE',  ( -1.000000000000000000, -0.000000000000000000, -0.000000000000000000 ) ) ;
#7944 = DIRECTION ( 'NONE',  ( 1.000000000000000000, -0.000000000000000000, -0.000000000000000000 ) ) ;
#7945 = DIRECTION ( 'NONE',  ( -1.000000000000000000, -0.000000000000000000, -0.000000000000000000 ) ) ;
#7946 = SHAPE_REPRESENTATION ( 'clamp', ( #6056 ), #12194 ) ;
#7947 = ORIENTED_EDGE ( 'NONE', *, *, #2538, .T. ) ;
#7948 = FACE_OUTER_BOUND ( 'NONE', #1373, .T. ) ;
#7949 = ADVANCED_FACE ( 'NONE', ( #7873, #11662 ), #159, .F. ) ;
#7950 = EDGE_CURVE ( 'NONE', #8654, #10725, #10538, .T. ) ;
#7951 = DIRECTION ( 'NONE',  ( 0.000000000000000000, 0.000000000000000000, -1.000000000000000000 ) ) ;
#7952 = DIRECTION ( 'NONE',  ( 1.000000000000000000, 0.000000000000000000, -0.000000000000000000 ) ) ;
#7953 = DIRECTION ( 'NONE',  ( 1.000000000000000000, 0.000000000000000000, 0.000000000000000000 ) ) ;
#7954 = DIRECTION ( 'NONE',  ( 0.000000000000000000, 0.000000000000000000, -1.000000000000000000 ) ) ;
#7955 = ORIENTED_EDGE ( 'NONE', *, *, #1801, .T. ) ;
#7956 = ORIENTED_EDGE ( 'NONE', *, *, #775, .F. ) ;
#7957 = CARTESIAN_POINT ( 'NONE',  ( 50.00005079999999680, 6.123233995736766282E-16, -5.000000000000000000 ) ) ;
#7958 = CARTESIAN_POINT ( 'NONE',  ( -25.00000000000000000, 0.000000000000000000, 0.000000000000000000 ) ) ;
#7959 = VERTEX_POINT ( 'NONE', #6686 ) ;
#7960 = CARTESIAN_POINT ( 'NONE',  ( 70.79898987322334847, 3.500000000000001332, -45.49999999999998579 ) ) ;
#7961 = VERTEX_POINT ( 'NONE', #2977 ) ;
#7962 = DIRECTION ( 'NONE',  ( -1.000000000000000000, -0.000000000000000000, -0.000000000000000000 ) ) ;
#7963 = VECTOR ( 'NONE', #10524, 1000.000000000000000 ) ;
#7964 = LINE ( 'NONE', #11884, #9602 ) ;
#7965 = DIRECTION ( 'NONE',  ( -1.000000000000000000, 0.000000000000000000, 0.000000000000000000 ) ) ;
#7966 = DIRECTION ( 'NONE',  ( 0.000000000000000000, 0.000000000000000000, 1.000000000000000000 ) ) ;
#7967 = CYLINDRICAL_SURFACE ( 'NONE', #2236, 9.600000000009600853 ) ;
#7968 = AXIS2_PLACEMENT_3D ( 'NONE', #10304, #9506, #9854 ) ;
#7969 = VECTOR ( 'NONE', #487, 1000.000000000000000 ) ;
#7970 = VERTEX_POINT ( 'NONE', #1225 ) ;
#7971 = ORIENTED_EDGE ( 'NONE', *, *, #6277, .F. ) ;
#7972 = CARTESIAN_POINT ( 'NONE',  ( 36.00000000000000711, -4.104405154062230115E-16, -2.224720805914714718E-17 ) ) ;
#7973 = ORIENTED_EDGE ( 'NONE', *, *, #5022, .T. ) ;
#7974 = EDGE_CURVE ( 'NONE', #2061, #10053, #5575, .T. ) ;
#7975 = CIRCLE ( 'NONE', #2569, 7.200000000007203305 ) ;
#7976 = AXIS2_PLACEMENT_3D ( 'NONE', #6552, #9621, #1872 ) ;
#7977 = PLANE ( 'NONE',  #9973 ) ;
#7978 = CLOSED_SHELL ( 'NONE', ( #6093, #5541, #6149, #676, #8463, #5897, #1344, #7078, #5038, #7475, #1138, #6603, #340 ) ) ;
#7979 = DIRECTION ( 'NONE',  ( -1.000000000000000000, -0.000000000000000000, -0.000000000000000000 ) ) ;
#7980 = CARTESIAN_POINT ( 'NONE',  ( 4.999999999999999112, -5.950465759858725612, -20.13931372320394786 ) ) ;
#7981 = DIRECTION ( 'NONE',  ( 0.000000000000000000, 0.000000000000000000, -1.000000000000000000 ) ) ;
#7982 = DIRECTION ( 'NONE',  ( 1.000000000000000000, 0.000000000000000000, 0.000000000000000000 ) ) ;
#7983 = ORIENTED_EDGE ( 'NONE', *, *, #5343, .T. ) ;
#7984 = CYLINDRICAL_SURFACE ( 'NONE', #5246, 20.24900000002024569 ) ;
#7985 = CIRCLE ( 'NONE', #9184, 5.000000000000000000 ) ;
#7986 = ORIENTED_EDGE ( 'NONE', *, *, #4227, .T. ) ;
#7987 = VECTOR ( 'NONE', #3620, 1000.000000000000000 ) ;
#7988 = EDGE_CURVE ( 'NONE', #7142, #6930, #3115, .T. ) ;
#7989 = ORIENTED_EDGE ( 'NONE', *, *, #5700, .T. ) ;
#7990 = AXIS2_PLACEMENT_3D ( 'NONE', #12268, #9834, #5658 ) ;
#7991 = DIRECTION ( 'NONE',  ( 0.000000000000000000, -1.000000000000000000, 0.000000000000000000 ) ) ;
#7992 = EDGE_CURVE ( 'NONE', #11981, #303, #4978, .T. ) ;
#7993 = CARTESIAN_POINT ( 'NONE',  ( 4.999999999999999112, 13.09267581720866858, 5.622796541391611669 ) ) ;
#7994 = ADVANCED_FACE ( 'NONE', ( #1928 ), #2921, .T. ) ;
#7995 = AXIS2_PLACEMENT_3D ( 'NONE', #6530, #9409, #583 ) ;
#7996 = CARTESIAN_POINT ( 'NONE',  ( -20.63749999999999929, 6.766173565289127388E-16, 5.525000000000000355 ) ) ;
#7997 = VECTOR ( 'NONE', #8181, 1000.000000000000000 ) ;
#7998 = ORIENTED_EDGE ( 'NONE', *, *, #8074, .F. ) ;
#7999 = DIRECTION ( 'NONE',  ( 0.000000000000000000, 0.000000000000000000, -1.000000000000000000 ) ) ;
#8000 = CARTESIAN_POINT ( 'NONE',  ( -20.00000000000000000, 3.061616997868383043E-15, -25.00000000000000000 ) ) ;
#8001 = EDGE_LOOP ( 'NONE', ( #2042, #12275, #1593, #1406 ) ) ;
#8002 = DIRECTION ( 'NONE',  ( 0.000000000000000000, 0.000000000000000000, -1.000000000000000000 ) ) ;
#8003 =( LENGTH_UNIT ( ) NAMED_UNIT ( * ) SI_UNIT ( .MILLI., .METRE. ) );
#8004 = CYLINDRICAL_SURFACE ( 'NONE', #5237, 7.200000000007202416 ) ;
#8005 = PRESENTATION_LAYER_ASSIGNMENT (  '', '', ( #7408 ) ) ;
#8006 = DIRECTION ( 'NONE',  ( -1.000000000000000000, -0.000000000000000000, -0.000000000000000000 ) ) ;
#8007 = ADVANCED_FACE ( 'NONE', ( #225 ), #4045, .T. ) ;
#8008 = CIRCLE ( 'NONE', #602, 5.750000000000000000 ) ;
#8010 = EDGE_CURVE ( 'NONE', #7624, #11240, #3920, .T. ) ;
#8009 = ORIENTED_EDGE ( 'NONE', *, *, #2548, .T. ) ;
#8011 = DIRECTION ( 'NONE',  ( 0.000000000000000000, 0.000000000000000000, -1.000000000000000000 ) ) ;
#8012 = CIRCLE ( 'NONE', #15, 0.1000000000000002554 ) ;
#8013 = EDGE_CURVE ( 'NONE', #10347, #8570, #10374, .T. ) ;
#8014 = DIRECTION ( 'NONE',  ( 1.000000000000000000, -0.000000000000000000, -0.000000000000000000 ) ) ;
#8015 = CIRCLE ( 'NONE', #9811, 9.600000000009600853 ) ;
#8016 = AXIS2_PLACEMENT_3D ( 'NONE', #8715, #5709, #2901 ) ;
#8017 = SURFACE_STYLE_FILL_AREA ( #9767 ) ;
#8018 = CYLINDRICAL_SURFACE ( 'NONE', #5810, 20.24900000002024569 ) ;
#8019 = AXIS2_PLACEMENT_3D ( 'NONE', #7688, #10611, #8554 ) ;
#8020 = AXIS2_PLACEMENT_3D ( 'NONE', #11516, #6785, #3720 ) ;
#8021 = TOROIDAL_SURFACE ( 'NONE', #2612, 2.690429798716874377, 1.199999999999999956 ) ;
#8022 = CARTESIAN_POINT ( 'NONE',  ( 36.00000000000000711, 0.000000000000000000, 0.000000000000000000 ) ) ;
#8023 = DIRECTION ( 'NONE',  ( 1.000000000000000000, 0.000000000000000000, 0.000000000000000000 ) ) ;
#8024 = VERTEX_POINT ( 'NONE', #2105 ) ;
#8025 = VERTEX_POINT ( 'NONE', #3864 ) ;
#8026 = LINE ( 'NONE', #2264, #11758 ) ;
#8027 = EDGE_CURVE ( 'NONE', #7435, #7808, #8796, .T. ) ;
#8028 = FACE_OUTER_BOUND ( 'NONE', #8325, .T. ) ;
#8029 = EDGE_CURVE ( 'NONE', #6360, #5264, #2793, .T. ) ;
#8030 = ORIENTED_EDGE ( 'NONE', *, *, #2971, .T. ) ;
#8031 = DIRECTION ( 'NONE',  ( 0.000000000000000000, 0.000000000000000000, -1.000000000000000000 ) ) ;
#8032 = PRODUCT_DEFINITION_CONTEXT ( 'detailed design', #3702, 'design' ) ;
#8033 = ORIENTED_EDGE ( 'NONE', *, *, #3117, .F. ) ;
#8034 = DIRECTION ( 'NONE',  ( -1.000000000000000000, 0.000000000000000000, -0.000000000000000000 ) ) ;
#8035 = PRESENTATION_LAYER_ASSIGNMENT (  '', '', ( #1028 ) ) ;
#8036 = AXIS2_PLACEMENT_3D ( 'NONE', #11898, #2340, #8169 ) ;
#8037 = AXIS2_PLACEMENT_3D ( 'NONE', #11564, #3019, #200 ) ;
#8038 = CIRCLE ( 'NONE', #2040, 8.099999999999999645 ) ;
#8039 = CARTESIAN_POINT ( 'NONE',  ( 4.999999999999999112, 22.37914155802285876, -2.791921004064323864 ) ) ;
#8040 = DIRECTION ( 'NONE',  ( 0.000000000000000000, 0.5000000000000009992, -0.8660254037844381525 ) ) ;
#8041 = VERTEX_POINT ( 'NONE', #1105 ) ;
#8042 = COLOUR_RGB ( '',1.000000000000000000, 0.9490196078431372140, 0.9098039215686274384 ) ;
#8043 = FACE_OUTER_BOUND ( 'NONE', #5502, .T. ) ;
#8044 = DIRECTION ( 'NONE',  ( 0.000000000000000000, 0.000000000000000000, -1.000000000000000000 ) ) ;
#8045 = VECTOR ( 'NONE', #6023, 1000.000000000000000 ) ;
#8046 = PRODUCT_DEFINITION_SHAPE ( 'NONE', 'NONE',  #8872 ) ;
#8047 = EDGE_LOOP ( 'NONE', ( #1632, #9661 ) ) ;
#8048 = EDGE_CURVE ( 'NONE', #8845, #7170, #3793, .T. ) ;
#8049 = CARTESIAN_POINT ( 'NONE',  ( -20.00000000000000000, 40.00000000000000711, -12.50000000000000000 ) ) ;
#8050 = ORIENTED_EDGE ( 'NONE', *, *, #2489, .T. ) ;
#8051 = DIRECTION ( 'NONE',  ( -0.000000000000000000, -1.000000000000000000, -0.000000000000000000 ) ) ;
#8052 = EDGE_LOOP ( 'NONE', ( #5698, #2129, #508, #4803, #8142, #8793 ) ) ;
#8053 = AXIS2_PLACEMENT_3D ( 'NONE', #5232, #3353, #11044 ) ;
#8054 = AXIS2_PLACEMENT_3D ( 'NONE', #11082, #703, #1830 ) ;
#8055 = VECTOR ( 'NONE', #10052, 1000.000000000000000 ) ;
#8056 = CIRCLE ( 'NONE', #12222, 9.600000000009600853 ) ;
#8057 = DIRECTION ( 'NONE',  ( 1.000000000000000000, 0.000000000000000000, 0.000000000000000000 ) ) ;
#8058 = CARTESIAN_POINT ( 'NONE',  ( 2.399999999999999467, 0.000000000000000000, 0.000000000000000000 ) ) ;
#8059 = PLANE ( 'NONE',  #3226 ) ;
#8060 = DIRECTION ( 'NONE',  ( -1.000000000000000000, 0.000000000000000000, 0.000000000000000000 ) ) ;
#8061 = DIRECTION ( 'NONE',  ( -0.000000000000000000, -0.000000000000000000, 1.000000000000000000 ) ) ;
#8062 = ORIENTED_EDGE ( 'NONE', *, *, #11948, .T. ) ;
#8063 = CARTESIAN_POINT ( 'NONE',  ( 2.399999999999999467, 0.000000000000000000, -4.000000000000000000 ) ) ;
#8064 = VECTOR ( 'NONE', #9893, 1000.000000000000000 ) ;
#8065 = ORIENTED_EDGE ( 'NONE', *, *, #2740, .T. ) ;
#8066 = CARTESIAN_POINT ( 'NONE',  ( 0.000000000000000000, 0.000000000000000000, 0.000000000000000000 ) ) ;
#8067 = CIRCLE ( 'NONE', #11640, 12.50000000000000000 ) ;
#8068 = VERTEX_POINT ( 'NONE', #9738 ) ;
#8069 = CARTESIAN_POINT ( 'NONE',  ( 0.000000000000000000, 6.123233995736766282E-16, -5.000000000000000000 ) ) ;
#8070 = CARTESIAN_POINT ( 'NONE',  ( 1.400000000000000133, 0.000000000000000000, 0.000000000000000000 ) ) ;
#8071 = LINE ( 'NONE', #11791, #7997 ) ;
#8072 = EDGE_CURVE ( 'NONE', #130, #7385, #5392, .T. ) ;
#8073 = AXIS2_PLACEMENT_3D ( 'NONE', #7891, #1179, #11799 ) ;
#8074 = EDGE_CURVE ( 'NONE', #11797, #11945, #3053, .T. ) ;
#8075 = ORIENTED_EDGE ( 'NONE', *, *, #10894, .T. ) ;
#8076 = CARTESIAN_POINT ( 'NONE',  ( -10.00000000000000000, 0.000000000000000000, 0.000000000000000000 ) ) ;
#8077 = ORIENTED_EDGE ( 'NONE', *, *, #10853, .T. ) ;
#8078 = DIRECTION ( 'NONE',  ( 0.000000000000000000, 0.000000000000000000, -1.000000000000000000 ) ) ;
#8079 = DIRECTION ( 'NONE',  ( -1.000000000000000000, -0.000000000000000000, -0.000000000000000000 ) ) ;
#8080 = AXIS2_PLACEMENT_3D ( 'NONE', #9111, #4392, #12078 ) ;
#8081 = VERTEX_POINT ( 'NONE', #4862 ) ;
#8082 = LINE ( 'NONE', #5070, #992 ) ;
#8083 = LINE ( 'NONE', #4184, #11762 ) ;
#8084 = EDGE_CURVE ( 'NONE', #4496, #10589, #2383, .T. ) ;
#8085 = CARTESIAN_POINT ( 'NONE',  ( -26.00000000000000355, 34.64101615137755630, 20.00000000000001066 ) ) ;
#8086 = CARTESIAN_POINT ( 'NONE',  ( 4.999999999999999112, -5.622796541391473113, -13.09267581720872720 ) ) ;
#8087 = EDGE_CURVE ( 'NONE', #12039, #11027, #1797, .T. ) ;
#8088 = AXIS2_PLACEMENT_3D ( 'NONE', #4138, #5135, #8099 ) ;
#8089 = EDGE_CURVE ( 'NONE', #2301, #10119, #5991, .T. ) ;
#8090 = CARTESIAN_POINT ( 'NONE',  ( 43.00000000000000000, -2.824006678639516377, 3.881363971466655904 ) ) ;
#8091 = DIRECTION ( 'NONE',  ( 0.000000000000000000, 0.4999999999999993339, -0.8660254037844390407 ) ) ;
#8092 = EDGE_CURVE ( 'NONE', #26, #2796, #6805, .T. ) ;
#8093 = VERTEX_POINT ( 'NONE', #1530 ) ;
#8094 = AXIS2_PLACEMENT_3D ( 'NONE', #7147, #10945, #6395 ) ;
#8095 = EDGE_LOOP ( 'NONE', ( #11257, #4078, #8643, #735 ) ) ;
#8096 = CARTESIAN_POINT ( 'NONE',  ( 4.799999999999999822, 0.000000000000000000, -1.000000000000000000 ) ) ;
#8097 = LINE ( 'NONE', #10832, #8045 ) ;
#8098 = ORIENTED_EDGE ( 'NONE', *, *, #10231, .F. ) ;
#8099 = DIRECTION ( 'NONE',  ( 0.000000000000000000, 0.000000000000000000, -1.000000000000000000 ) ) ;
#8100 = EDGE_LOOP ( 'NONE', ( #3706, #11512, #9809, #4872 ) ) ;
#8101 = CARTESIAN_POINT ( 'NONE',  ( -31.74999999999995737, 0.000000000000000000, 0.000000000000000000 ) ) ;
#8102 = EDGE_CURVE ( 'NONE', #11745, #4049, #197, .T. ) ;
#8103 = FACE_OUTER_BOUND ( 'NONE', #2263, .T. ) ;
#8104 = LINE ( 'NONE', #10844, #2168 ) ;
#8105 = CARTESIAN_POINT ( 'NONE',  ( 36.00000000000000711, -2.432816653220593039, 4.137801726981678030 ) ) ;
#8106 = CARTESIAN_POINT ( 'NONE',  ( 0.000000000000000000, -8.872489362018088244, -14.40062958310474883 ) ) ;
#8107 = VERTEX_POINT ( 'NONE', #3347 ) ;
#8108 = AXIS2_PLACEMENT_3D ( 'NONE', #6124, #3943, #8895 ) ;
#8109 = DIRECTION ( 'NONE',  ( 1.000000000000000000, 0.000000000000000000, 0.000000000000000000 ) ) ;
#8110 = ORIENTED_EDGE ( 'NONE', *, *, #7689, .F. ) ;
#8111 = DIRECTION ( 'NONE',  ( 0.000000000000000000, 1.000000000000000000, -1.224646799147353207E-16 ) ) ;
#8112 = ORIENTED_EDGE ( 'NONE', *, *, #3623, .F. ) ;
#8113 = ADVANCED_FACE ( 'NONE', ( #3405 ), #399, .T. ) ;
#8114 = EDGE_CURVE ( 'NONE', #474, #3672, #6187, .T. ) ;
#8115 = DIRECTION ( 'NONE',  ( 0.000000000000000000, 0.000000000000000000, 1.000000000000000000 ) ) ;
#8116 = DIRECTION ( 'NONE',  ( 0.000000000000000000, 0.5000000000000008882, -0.8660254037844381525 ) ) ;
#8117 = CARTESIAN_POINT ( 'NONE',  ( 4.999999999999999112, -13.09267581720870766, 5.622796541391519298 ) ) ;
#8118 = CARTESIAN_POINT ( 'NONE',  ( 4.999999999999999112, -16.90755573046746463, 0.4834863907625160939 ) ) ;
#8119 = ORIENTED_EDGE ( 'NONE', *, *, #8240, .T. ) ;
#8120 = DIRECTION ( 'NONE',  ( -1.000000000000000000, 0.000000000000000000, 0.000000000000000000 ) ) ;
#8121 = VERTEX_POINT ( 'NONE', #6977 ) ;
#8122 =( LENGTH_UNIT ( ) NAMED_UNIT ( * ) SI_UNIT ( .MILLI., .METRE. ) );
#8123 = EDGE_LOOP ( 'NONE', ( #8307, #6943, #7105, #5673 ) ) ;
#8124 = DIRECTION ( 'NONE',  ( 0.000000000000000000, 0.000000000000000000, -1.000000000000000000 ) ) ;
#8125 = DIRECTION ( 'NONE',  ( -1.000000000000000000, 0.000000000000000000, 0.000000000000000000 ) ) ;
#8126 = EDGE_LOOP ( 'NONE', ( #5780, #9941, #3734, #11249 ) ) ;
#8127 = CARTESIAN_POINT ( 'NONE',  ( 0.000000000000000000, -5.622796541391473113, -13.09267581720872720 ) ) ;
#8128 = ORIENTED_EDGE ( 'NONE', *, *, #7230, .F. ) ;
#8129 = DIRECTION ( 'NONE',  ( 0.000000000000000000, 0.000000000000000000, 1.000000000000000000 ) ) ;
#8130 = ORIENTED_EDGE ( 'NONE', *, *, #1332, .F. ) ;
#8131 =( LENGTH_UNIT ( ) NAMED_UNIT ( * ) SI_UNIT ( .MILLI., .METRE. ) );
#8132 = DIRECTION ( 'NONE',  ( 0.000000000000000000, 0.000000000000000000, 1.000000000000000000 ) ) ;
#8133 = EDGE_LOOP ( 'NONE', ( #7103, #11156, #444, #7265 ) ) ;
#8134 = DIRECTION ( 'NONE',  ( -0.000000000000000000, 0.8660254037844390407, 0.4999999999999993339 ) ) ;
#8135 = ADVANCED_FACE ( 'NONE', ( #1286 ), #9974, .T. ) ;
#8136 = PRESENTATION_STYLE_ASSIGNMENT (( #1366 ) ) ;
#8137 = CYLINDRICAL_SURFACE ( 'NONE', #9626, 5.000000000000004441 ) ;
#8138 = CARTESIAN_POINT ( 'NONE',  ( -20.00000000000000000, 0.000000000000000000, 0.000000000000000000 ) ) ;
#8139 = DIRECTION ( 'NONE',  ( 0.000000000000000000, 0.000000000000000000, 1.000000000000000000 ) ) ;
#8140 = DIRECTION ( 'NONE',  ( -1.000000000000000000, 0.000000000000000000, 0.000000000000000000 ) ) ;
#8141 = ORIENTED_EDGE ( 'NONE', *, *, #11197, .T. ) ;
#8142 = ORIENTED_EDGE ( 'NONE', *, *, #7444, .F. ) ;
#8143 = DIRECTION ( 'NONE',  ( -1.000000000000000000, -0.000000000000000000, -0.000000000000000000 ) ) ;
#8144 = CARTESIAN_POINT ( 'NONE',  ( 37.00000000000000711, -4.104405154062230115E-16, -2.224720805914714718E-17 ) ) ;
#8145 = ORIENTED_EDGE ( 'NONE', *, *, #6474, .F. ) ;
#8146 = CARTESIAN_POINT ( 'NONE',  ( 2.500000000000000000, 0.000000000000000000, 0.000000000000000000 ) ) ;
#8147 = EDGE_CURVE ( 'NONE', #9896, #2664, #11370, .T. ) ;
#8148 = ORIENTED_EDGE ( 'NONE', *, *, #9065, .T. ) ;
#8149 = DIRECTION ( 'NONE',  ( 0.000000000000000000, 0.000000000000000000, 1.000000000000000000 ) ) ;
#8150 = ADVANCED_FACE ( 'NONE', ( #6228 ), #11712, .T. ) ;
#8151 = EDGE_CURVE ( 'NONE', #10787, #8093, #10963, .T. ) ;
#8152 = ORIENTED_EDGE ( 'NONE', *, *, #12250, .F. ) ;
#8153 = CARTESIAN_POINT ( 'NONE',  ( 0.000000000000000000, 17.79862902732265084, 13.85025647830063100 ) ) ;
#8154 = FACE_OUTER_BOUND ( 'NONE', #7049, .T. ) ;
#8155 = CARTESIAN_POINT ( 'NONE',  ( 36.00000000000000711, 34.64101615137756340, -19.99999999999998934 ) ) ;
#8156 = VERTEX_POINT ( 'NONE', #6157 ) ;
#8157 = DIRECTION ( 'NONE',  ( 0.000000000000000000, -1.000000000000000000, 1.287488025362403787E-15 ) ) ;
#8158 = CARTESIAN_POINT ( 'NONE',  ( 45.00000000000000000, 0.000000000000000000, 5.000000000000000000 ) ) ;
#8159 = ORIENTED_EDGE ( 'NONE', *, *, #7144, .T. ) ;
#8160 = DIRECTION ( 'NONE',  ( 0.000000000000000000, 0.000000000000000000, 1.000000000000000000 ) ) ;
#8161 = UNCERTAINTY_MEASURE_WITH_UNIT (LENGTH_MEASURE( 1.000000000000000082E-05 ), #425, 'distance_accuracy_value', 'NONE');
#8162 = ORIENTED_EDGE ( 'NONE', *, *, #6663, .F. ) ;
#8163 = PRODUCT_RELATED_PRODUCT_CATEGORY ( 'part', '', ( #5415 ) ) ;
#8164 = DIRECTION ( 'NONE',  ( 0.000000000000000000, 0.8660254037844362651, 0.5000000000000038858 ) ) ;
#8165 = LINE ( 'NONE', #8875, #5190 ) ;
#8166 = PLANE ( 'NONE',  #3029 ) ;
#8167 = AXIS2_PLACEMENT_3D ( 'NONE', #1881, #6854, #7702 ) ;
#8168 = CIRCLE ( 'NONE', #4557, 9.600000000009599077 ) ;
#8169 = DIRECTION ( 'NONE',  ( 0.000000000000000000, 0.000000000000000000, 1.000000000000000000 ) ) ;
#8170 = FACE_OUTER_BOUND ( 'NONE', #2678, .T. ) ;
#8171 = ORIENTED_EDGE ( 'NONE', *, *, #8767, .F. ) ;
#8172 = LINE ( 'NONE', #2475, #3064 ) ;
#8173 = ORIENTED_EDGE ( 'NONE', *, *, #5267, .T. ) ;
#8174 = EDGE_CURVE ( 'NONE', #7438, #5310, #1477, .T. ) ;
#8176 = ADVANCED_FACE ( 'NONE', ( #4104 ), #4337, .T. ) ;
#8175 = EDGE_LOOP ( 'NONE', ( #11438, #7175, #7520 ) ) ;
#8178 = CARTESIAN_POINT ( 'NONE',  ( 4.999999999999997335, 6.799999999999999822, 1.500000000000000000 ) ) ;
#8177 = AXIS2_PLACEMENT_3D ( 'NONE', #10917, #12041, #7314 ) ;
#8179 = DIRECTION ( 'NONE',  ( 0.000000000000000000, 0.000000000000000000, 1.000000000000000000 ) ) ;
#8180 = ORIENTED_EDGE ( 'NONE', *, *, #9866, .T. ) ;
#8181 = DIRECTION ( 'NONE',  ( -0.000000000000000000, -0.000000000000000000, 1.000000000000000000 ) ) ;
#8182 = CIRCLE ( 'NONE', #1186, 21.00000000002100009 ) ;
#8183 = ORIENTED_EDGE ( 'NONE', *, *, #135, .F. ) ;
#8184 = CLOSED_SHELL ( 'NONE', ( #1834, #527, #3320, #8673, #5633, #271, #6550, #6424, #4856, #6336, #1330, #6469, #2257, #1977, #6763, #11076, #4550, #6841, #220, #7152, #4633, #3951, #8904, #6631, #327, #4696, #9334 ) ) ;
#8185 = DIRECTION ( 'NONE',  ( -1.000000000000000000, -0.000000000000000000, 0.000000000000000000 ) ) ;
#8186 = EDGE_LOOP ( 'NONE', ( #10861, #1247, #2639, #7998 ) ) ;
#8187 = CARTESIAN_POINT ( 'NONE',  ( 51.00000000000000000, 0.000000000000000000, 0.000000000000000000 ) ) ;
#8188 = VERTEX_POINT ( 'NONE', #5291 ) ;
#8189 = DIRECTION ( 'NONE',  ( -1.000000000000000000, 0.000000000000000000, -0.000000000000000000 ) ) ;
#8190 = AXIS2_PLACEMENT_3D ( 'NONE', #9166, #6479, #7412 ) ;
#8191 = PRESENTATION_LAYER_ASSIGNMENT (  '', '', ( #4588 ) ) ;
#8192 = CARTESIAN_POINT ( 'NONE',  ( 0.5000000000000000000, -6.429618962271402616, 0.000000000000000000 ) ) ;
#8193 = CARTESIAN_POINT ( 'NONE',  ( 0.7251148409942000939, 0.5999999999999998668, 3.753893533104442071 ) ) ;
#8194 = FACE_OUTER_BOUND ( 'NONE', #9023, .T. ) ;
#8195 = DIRECTION ( 'NONE',  ( 0.000000000000000000, -0.7071067811865389130, -0.7071067811865561215 ) ) ;
#8196 = CARTESIAN_POINT ( 'NONE',  ( 0.000000000000000000, 22.37914155802285876, 6.808078995945277434 ) ) ;
#8197 = AXIS2_PLACEMENT_3D ( 'NONE', #8039, #11759, #11935 ) ;
#8198 = ORIENTED_EDGE ( 'NONE', *, *, #11525, .T. ) ;
#8199 = ORIENTED_EDGE ( 'NONE', *, *, #5139, .T. ) ;
#8200 = CARTESIAN_POINT ( 'NONE',  ( 0.1890552205643245831, -0.5999999999999995337, -3.298086786345711285 ) ) ;
#8201 = CIRCLE ( 'NONE', #10417, 2.500000000000002220 ) ;
#8202 = CARTESIAN_POINT ( 'NONE',  ( 2.499999999999998668, 4.916402349214582301, 20.41639017900861219 ) ) ;
#8203 = AXIS2_PLACEMENT_3D ( 'NONE', #11726, #4235, #4350 ) ;
#8204 = ORIENTED_EDGE ( 'NONE', *, *, #4489, .T. ) ;
#8205 = DIRECTION ( 'NONE',  ( 0.000000000000000000, 0.000000000000000000, 1.000000000000000000 ) ) ;
#8206 = EDGE_LOOP ( 'NONE', ( #5331, #11618, #7574, #1144 ) ) ;
#8207 = CARTESIAN_POINT ( 'NONE',  ( 46.00000000000000000, 3.500000000000001332, -38.49999999999998579 ) ) ;
#8208 = VECTOR ( 'NONE', #10382, 1000.000000000000000 ) ;
#8209 = AXIS2_PLACEMENT_3D ( 'NONE', #3011, #5951, #370 ) ;
#8210 = VECTOR ( 'NONE', #8308, 1000.000000000000000 ) ;
#8211 = CARTESIAN_POINT ( 'NONE',  ( 0.000000000000000000, 0.000000000000000000, 0.000000000000000000 ) ) ;
#8212 = DIRECTION ( 'NONE',  ( -1.000000000000000000, 9.497745524640252240E-18, 1.039762770660628461E-17 ) ) ;
#8213 = EDGE_CURVE ( 'NONE', #11053, #3803, #1401, .T. ) ;
#8214 = CARTESIAN_POINT ( 'NONE',  ( 4.999999999999999112, 0.000000000000000000, 0.000000000000000000 ) ) ;
#8215 = CARTESIAN_POINT ( 'NONE',  ( 36.00000000000000711, 12.50000000000000000, -37.99671038392666134 ) ) ;
#8216 = EDGE_LOOP ( 'NONE', ( #5552, #9495, #2868, #5693, #1853, #2871, #3749, #9264, #6844, #9122, #4878, #5473, #8433, #747, #8971, #10731, #623, #3530, #11719, #12340, #7122, #1805, #5077, #10194, #1769, #3579, #5968, #2229, #4977, #2357, #6167, #6779, #7877, #4972, #10020, #3851, #874, #11307, #1579, #10592, #11262, #6883, #10749, #6279, #289, #8458, #7343, #1978, #4505, #1669, #4461, #10740, #357, #232, #8662, #4785, #12077, #10410, #5281, #6073, #1393, #11717, #7212, #5961, #5272, #845, #7089, #3330, #7811 ) ) ;
#8217 = EDGE_CURVE ( 'NONE', #9456, #3968, #12165, .T. ) ;
#8218 = CARTESIAN_POINT ( 'NONE',  ( -10.00000000000000000, 0.000000000000000000, 0.000000000000000000 ) ) ;
#8219 = LINE ( 'NONE', #8158, #9822 ) ;
#8220 =( GEOMETRIC_REPRESENTATION_CONTEXT ( 3 ) GLOBAL_UNCERTAINTY_ASSIGNED_CONTEXT ( ( #3905 ) ) GLOBAL_UNIT_ASSIGNED_CONTEXT ( ( #1917, #5782, #97 ) ) REPRESENTATION_CONTEXT ( 'NONE', 'WORKASPACE' ) );
#8221 = CIRCLE ( 'NONE', #2219, 27.00000000002699707 ) ;
#8222 = EDGE_LOOP ( 'NONE', ( #2716, #2689, #1526, #2291 ) ) ;
#8223 = CYLINDRICAL_SURFACE ( 'NONE', #3894, 9.600000000009597301 ) ;
#8224 = VECTOR ( 'NONE', #11140, 1000.000000000000000 ) ;
#8225 = AXIS2_PLACEMENT_3D ( 'NONE', #1108, #4919, #8803 ) ;
#8226 = ORIENTED_EDGE ( 'NONE', *, *, #3058, .T. ) ;
#8227 = CIRCLE ( 'NONE', #10811, 7.399999999999999467 ) ;
#8228 = DIRECTION ( 'NONE',  ( 0.000000000000000000, 0.000000000000000000, -1.000000000000000000 ) ) ;
#8229 = PRESENTATION_LAYER_ASSIGNMENT (  '', '', ( #8831 ) ) ;
#8230 = VECTOR ( 'NONE', #11763, 999.9999999999998863 ) ;
#8231 = AXIS2_PLACEMENT_3D ( 'NONE', #11310, #2626, #11126 ) ;
#8232 = FACE_OUTER_BOUND ( 'NONE', #9395, .T. ) ;
#8233 = DIRECTION ( 'NONE',  ( 0.000000000000000000, 0.000000000000000000, 1.000000000000000000 ) ) ;
#8234 = AXIS2_PLACEMENT_3D ( 'NONE', #7241, #1533, #3481 ) ;
#8235 = AXIS2_PLACEMENT_3D ( 'NONE', #6542, #9724, #4954 ) ;
#8236 = DIRECTION ( 'NONE',  ( 0.000000000000000000, 0.000000000000000000, -1.000000000000000000 ) ) ;
#8237 = LINE ( 'NONE', #6482, #3820 ) ;
#8238 = EDGE_LOOP ( 'NONE', ( #8381, #10686, #2798, #10957 ) ) ;
#8239 = EDGE_CURVE ( 'NONE', #10725, #7180, #8165, .T. ) ;
#8240 = EDGE_CURVE ( 'NONE', #279, #10710, #3003, .T. ) ;
#8241 = CARTESIAN_POINT ( 'NONE',  ( 0.000000000000000000, -18.05452603534171985, 9.168210874537514599 ) ) ;
#8242 = EDGE_CURVE ( 'NONE', #6431, #10717, #5153, .T. ) ;
#8243 = EDGE_LOOP ( 'NONE', ( #5942, #6918, #1785, #1720 ) ) ;
#8244 = CYLINDRICAL_SURFACE ( 'NONE', #1671, 14.24900000001425227 ) ;
#8245 = DIRECTION ( 'NONE',  ( 0.000000000000000000, 0.000000000000000000, 1.000000000000000000 ) ) ;
#8246 = ORIENTED_EDGE ( 'NONE', *, *, #10117, .F. ) ;
#8247 = CIRCLE ( 'NONE', #2842, 4.250000000000000000 ) ;
#8248 = DIRECTION ( 'NONE',  ( 0.000000000000000000, 0.000000000000000000, 1.000000000000000000 ) ) ;
#8249 = AXIS2_PLACEMENT_3D ( 'NONE', #3889, #6895, #9513 ) ;
#8250 = CIRCLE ( 'NONE', #647, 7.200000000007202416 ) ;
#8251 = CARTESIAN_POINT ( 'NONE',  ( 26.00000000000000355, 6.123233995736773185E-16, -46.99999999999999289 ) ) ;
#8252 = VERTEX_POINT ( 'NONE', #6346 ) ;
#8253 = CARTESIAN_POINT ( 'NONE',  ( 0.000000000000000000, 8.872489362018189496, 14.40062958310468666 ) ) ;
#8254 = ADVANCED_FACE ( 'NONE', ( #8232 ), #12027, .T. ) ;
#8255 = EDGE_CURVE ( 'NONE', #12042, #8435, #4053, .T. ) ;
#8256 = AXIS2_PLACEMENT_3D ( 'NONE', #10014, #5952, #8838 ) ;
#8257 = AXIS2_PLACEMENT_3D ( 'NONE', #7540, #11155, #2590 ) ;
#8258 = VERTEX_POINT ( 'NONE', #9236 ) ;
#8259 = AXIS2_PLACEMENT_3D ( 'NONE', #8509, #6705, #2806 ) ;
#8260 = LINE ( 'NONE', #10985, #984 ) ;
#8261 = ORIENTED_EDGE ( 'NONE', *, *, #7000, .T. ) ;
#8262 = CARTESIAN_POINT ( 'NONE',  ( 46.00000000000000000, -5.000000000000004441, -41.99999999999998579 ) ) ;
#8263 = VERTEX_POINT ( 'NONE', #1773 ) ;
#8264 = CARTESIAN_POINT ( 'NONE',  ( 0.000000000000000000, 15.57980286237472889, 22.05152472667135655 ) ) ;
#8265 = CIRCLE ( 'NONE', #9867, 5.000000000000000000 ) ;
#8266 = LINE ( 'NONE', #5445, #1199 ) ;
#8267 = EDGE_CURVE ( 'NONE', #5277, #10549, #8292, .T. ) ;
#8268 = DIRECTION ( 'NONE',  ( 0.000000000000000000, 0.5000000000000008882, -0.8660254037844381525 ) ) ;
#8269 = DIRECTION ( 'NONE',  ( 0.000000000000000000, 0.000000000000000000, -1.000000000000000000 ) ) ;
#8270 = DIRECTION ( 'NONE',  ( 0.000000000000000000, 0.000000000000000000, -1.000000000000000000 ) ) ;
#8271 = EDGE_LOOP ( 'NONE', ( #742, #1635, #12325, #4765 ) ) ;
#8272 = EDGE_LOOP ( 'NONE', ( #6468, #6287, #8077, #12143 ) ) ;
#8273 = DIRECTION ( 'NONE',  ( 1.000000000000000000, 3.903127820947815962E-18, 0.000000000000000000 ) ) ;
#8274 = CIRCLE ( 'NONE', #869, 7.200000000007202416 ) ;
#8275 = DIRECTION ( 'NONE',  ( 1.000000000000000000, -0.000000000000000000, 0.000000000000000000 ) ) ;
#8276 = ORIENTED_EDGE ( 'NONE', *, *, #7064, .T. ) ;
#8277 = DIRECTION ( 'NONE',  ( 0.000000000000000000, 0.000000000000000000, -1.000000000000000000 ) ) ;
#8278 = ORIENTED_EDGE ( 'NONE', *, *, #8533, .F. ) ;
#8279 = FACE_OUTER_BOUND ( 'NONE', #6103, .T. ) ;
#8280 = CARTESIAN_POINT ( 'NONE',  ( 2.499999999999999556, 14.41081992069310225, 22.83261415639507419 ) ) ;
#8281 = CYLINDRICAL_SURFACE ( 'NONE', #8054, 9.600000000009600853 ) ;
#8282 = DIRECTION ( 'NONE',  ( 1.000000000000000000, -0.000000000000000000, -0.000000000000000000 ) ) ;
#8283 = ORIENTED_EDGE ( 'NONE', *, *, #11584, .F. ) ;
#8284 = DIRECTION ( 'NONE',  ( 1.000000000000000000, -0.000000000000000000, -0.000000000000000000 ) ) ;
#8285 = CARTESIAN_POINT ( 'NONE',  ( 0.000000000000000000, 0.000000000000000000, 0.000000000000000000 ) ) ;
#8286 = ORIENTED_EDGE ( 'NONE', *, *, #946, .F. ) ;
#8287 = CARTESIAN_POINT ( 'NONE',  ( 0.000000000000000000, 0.4834863907628118573, -16.90755573046745397 ) ) ;
#8288 = AXIS2_PLACEMENT_3D ( 'NONE', #7960, #2319, #3212 ) ;
#8289 = VERTEX_POINT ( 'NONE', #1589 ) ;
#8290 = ADVANCED_FACE ( 'NONE', ( #11276 ), #11215, .T. ) ;
#8291 = ADVANCED_FACE ( 'NONE', ( #6593 ), #10275, .T. ) ;
#8292 = LINE ( 'NONE', #656, #3203 ) ;
#8293 = FACE_OUTER_BOUND ( 'NONE', #503, .T. ) ;
#8294 = VECTOR ( 'NONE', #11311, 1000.000000000000000 ) ;
#8295 = DIRECTION ( 'NONE',  ( -1.000000000000000000, 0.000000000000000000, 0.000000000000000000 ) ) ;
#8296 = CARTESIAN_POINT ( 'NONE',  ( 4.078421086530217288, -3.990950201428958621, -1.000000000000000000 ) ) ;
#8297 = VERTEX_POINT ( 'NONE', #8479 ) ;
#8298 = DIRECTION ( 'NONE',  ( 0.000000000000000000, 0.000000000000000000, 1.000000000000000000 ) ) ;
#8299 = ORIENTED_EDGE ( 'NONE', *, *, #6959, .T. ) ;
#8300 = DIRECTION ( 'NONE',  ( 0.000000000000000000, 0.000000000000000000, 1.000000000000000000 ) ) ;
#8301 = ORIENTED_EDGE ( 'NONE', *, *, #10995, .T. ) ;
#8302 = CARTESIAN_POINT ( 'NONE',  ( 46.00000000000000000, 3.500000000000001332, -38.49999999999998579 ) ) ;
#8303 = EDGE_CURVE ( 'NONE', #11016, #1740, #3478, .T. ) ;
#8304 = LINE ( 'NONE', #4482, #1364 ) ;
#8305 = ADVANCED_FACE ( 'NONE', ( #11149 ), #10330, .T. ) ;
#8306 = ADVANCED_FACE ( 'NONE', ( #10156 ), #4469, .F. ) ;
#8307 = ORIENTED_EDGE ( 'NONE', *, *, #10535, .F. ) ;
#8308 = DIRECTION ( 'NONE',  ( -0.000000000000000000, -1.000000000000000000, -0.000000000000000000 ) ) ;
#8309 = ORIENTED_EDGE ( 'NONE', *, *, #6476, .F. ) ;
#8310 = FACE_OUTER_BOUND ( 'NONE', #2849, .T. ) ;
#8311 = ORIENTED_EDGE ( 'NONE', *, *, #886, .T. ) ;
#8312 = SURFACE_STYLE_FILL_AREA ( #607 ) ;
#8313 = DIRECTION ( 'NONE',  ( -1.000000000000000000, -0.000000000000000000, -0.000000000000000000 ) ) ;
#8314 = ORIENTED_EDGE ( 'NONE', *, *, #6887, .F. ) ;
#8315 = DIRECTION ( 'NONE',  ( -1.000000000000000000, 0.000000000000000000, 0.000000000000000000 ) ) ;
#8316 = PRODUCT_RELATED_PRODUCT_CATEGORY ( 'part', '', ( #3037 ) ) ;
#8317 = CARTESIAN_POINT ( 'NONE',  ( 0.000000000000000000, 0.000000000000000000, 0.000000000000000000 ) ) ;
#8318 = CARTESIAN_POINT ( 'NONE',  ( 36.00000000000000000, 30.00000000000000711, 20.00000000000001066 ) ) ;
#8319 = DIRECTION ( 'NONE',  ( -1.000000000000000000, -0.000000000000000000, 0.000000000000000000 ) ) ;
#8320 = ORIENTED_EDGE ( 'NONE', *, *, #4164, .F. ) ;
#8321 = VERTEX_POINT ( 'NONE', #10220 ) ;
#8322 = CARTESIAN_POINT ( 'NONE',  ( 0.4784740205221562626, -0.5999999999999993117, -3.610260709030697956 ) ) ;
#8323 = FILL_AREA_STYLE ('',( #6326 ) ) ;
#8324 = CARTESIAN_POINT ( 'NONE',  ( -10.00000000000000000, 0.000000000000000000, 0.000000000000000000 ) ) ;
#8325 = EDGE_LOOP ( 'NONE', ( #4531, #7418, #10236, #856, #11562, #9720, #4293, #973, #6692, #6674, #320, #11029 ) ) ;
#8326 = CARTESIAN_POINT ( 'NONE',  ( -20.00000000000000000, 44.00000000000001421, 12.50000000000000000 ) ) ;
#8327 = EDGE_CURVE ( 'NONE', #10119, #331, #11326, .T. ) ;
#8328 = VERTEX_POINT ( 'NONE', #714 ) ;
#8329 = LINE ( 'NONE', #3573, #6231 ) ;
#8330 = ADVANCED_FACE ( 'NONE', ( #4526 ), #4662, .T. ) ;
#8331 = CARTESIAN_POINT ( 'NONE',  ( 2.499999999999999556, 22.83261415639503156, 14.41081992069317330 ) ) ;
#8332 = DIRECTION ( 'NONE',  ( -1.000000000000000000, 0.000000000000000000, 0.000000000000000000 ) ) ;
#8333 = ORIENTED_EDGE ( 'NONE', *, *, #5630, .F. ) ;
#8334 = DIRECTION ( 'NONE',  ( -0.000000000000000000, -0.000000000000000000, -1.000000000000000000 ) ) ;
#8335 = CARTESIAN_POINT ( 'NONE',  ( 4.999999999999999112, -21.74405275335762155, 5.984728032764886407 ) ) ;
#8336 = ORIENTED_EDGE ( 'NONE', *, *, #11296, .F. ) ;
#8337 = FACE_OUTER_BOUND ( 'NONE', #7584, .T. ) ;
#8338 = DIRECTION ( 'NONE',  ( 0.000000000000000000, 0.000000000000000000, -1.000000000000000000 ) ) ;
#8339 = ORIENTED_EDGE ( 'NONE', *, *, #4179, .F. ) ;
#8340 = DIRECTION ( 'NONE',  ( -1.000000000000000000, 0.000000000000000000, 0.000000000000000000 ) ) ;
#8341 = ORIENTED_EDGE ( 'NONE', *, *, #5526, .F. ) ;
#8342 =( NAMED_UNIT ( * ) PLANE_ANGLE_UNIT ( ) SI_UNIT ( $, .RADIAN. ) );
#8343 = CARTESIAN_POINT ( 'NONE',  ( 4.999999999999999112, -21.74405275335762155, 5.984728032764886407 ) ) ;
#8344 = DIRECTION ( 'NONE',  ( 0.000000000000000000, 0.000000000000000000, -1.000000000000000000 ) ) ;
#8345 = CARTESIAN_POINT ( 'NONE',  ( 4.999999999999999112, -13.85025647830069317, 17.79862902732260110 ) ) ;
#8346 = DIRECTION ( 'NONE',  ( 0.000000000000000000, -0.7071067811865389130, -0.7071067811865561215 ) ) ;
#8347 = ORIENTED_EDGE ( 'NONE', *, *, #1272, .F. ) ;
#8348 = ORIENTED_EDGE ( 'NONE', *, *, #7107, .F. ) ;
#8349 = CARTESIAN_POINT ( 'NONE',  ( 36.00000000000000711, -2.172883482918394282, 4.280020720704565740 ) ) ;
#8350 = EDGE_LOOP ( 'NONE', ( #2201, #4578, #11366, #6509 ) ) ;
#8351 = CYLINDRICAL_SURFACE ( 'NONE', #9666, 9.600000000009600853 ) ;
#8352 = ADVANCED_FACE ( 'NONE', ( #5476 ), #2657, .T. ) ;
#8353 = SHAPE_DEFINITION_REPRESENTATION ( #10622, #1544 ) ;
#8354 = VERTEX_POINT ( 'NONE', #9295 ) ;
#8355 = LINE ( 'NONE', #11337, #3402 ) ;
#8356 = DIRECTION ( 'NONE',  ( -1.000000000000000000, 0.000000000000000000, 0.000000000000000000 ) ) ;
#8357 = VECTOR ( 'NONE', #3180, 1000.000000000000000 ) ;
#8358 = CIRCLE ( 'NONE', #10944, 9.600000000009600853 ) ;
#8359 = ORIENTED_EDGE ( 'NONE', *, *, #4394, .F. ) ;
#8360 = CARTESIAN_POINT ( 'NONE',  ( 4.999999999999999112, 0.000000000000000000, 0.000000000000000000 ) ) ;
#8361 = EDGE_CURVE ( 'NONE', #1155, #7542, #12135, .T. ) ;
#8362 = ORIENTED_EDGE ( 'NONE', *, *, #5993, .T. ) ;
#8363 = CARTESIAN_POINT ( 'NONE',  ( 45.00000000000001421, 50.00000000000000711, -46.00000000000000000 ) ) ;
#8364 = VECTOR ( 'NONE', #3675, 1000.000000000000000 ) ;
#8365 = ORIENTED_EDGE ( 'NONE', *, *, #3596, .F. ) ;
#8366 = AXIS2_PLACEMENT_3D ( 'NONE', #5062, #11795, #8890 ) ;
#8367 = EDGE_CURVE ( 'NONE', #10792, #5917, #2585, .T. ) ;
#8368 = PRESENTATION_STYLE_ASSIGNMENT (( #2928 ) ) ;
#8369 = EDGE_CURVE ( 'NONE', #5296, #11243, #1662, .T. ) ;
#8370 = CARTESIAN_POINT ( 'NONE',  ( 4.999999999999999112, 0.000000000000000000, 0.000000000000000000 ) ) ;
#8371 = ORIENTED_EDGE ( 'NONE', *, *, #1269, .F. ) ;
#8372 = DIRECTION ( 'NONE',  ( 0.000000000000000000, -0.3826834323650773473, -0.9238795325112919565 ) ) ;
#8373 = AXIS2_PLACEMENT_3D ( 'NONE', #8713, #6084, #9843 ) ;
#8374 = CIRCLE ( 'NONE', #1173, 9.600000000009600853 ) ;
#8375 = LINE ( 'NONE', #7326, #4183 ) ;
#8376 = VECTOR ( 'NONE', #1529, 1000.000000000000000 ) ;
#8377 = ADVANCED_FACE ( 'NONE', ( #3662 ), #7479, .T. ) ;
#8378 = CYLINDRICAL_SURFACE ( 'NONE', #10841, 7.500000000000000888 ) ;
#8379 = DIRECTION ( 'NONE',  ( 1.000000000000000000, -0.000000000000000000, 0.000000000000000000 ) ) ;
#8380 = ORIENTED_EDGE ( 'NONE', *, *, #5183, .T. ) ;
#8381 = ORIENTED_EDGE ( 'NONE', *, *, #9742, .F. ) ;
#8382 = DIRECTION ( 'NONE',  ( 0.000000000000000000, 0.000000000000000000, 1.000000000000000000 ) ) ;
#8383 = EDGE_CURVE ( 'NONE', #1305, #474, #3602, .T. ) ;
#8384 = DIRECTION ( 'NONE',  ( 0.000000000000000000, 1.000000000000000000, 3.614007241614734605E-15 ) ) ;
#8385 = EDGE_CURVE ( 'NONE', #7662, #5192, #6670, .T. ) ;
#8386 = EDGE_CURVE ( 'NONE', #6597, #6982, #8535, .T. ) ;
#8387 = AXIS2_PLACEMENT_3D ( 'NONE', #10515, #12192, #1900 ) ;
#8388 = FACE_BOUND ( 'NONE', #1104, .T. ) ;
#8389 = VECTOR ( 'NONE', #4001, 1000.000000000000000 ) ;
#8390 = EDGE_LOOP ( 'NONE', ( #11551, #6644, #6489, #7276 ) ) ;
#8391 = CARTESIAN_POINT ( 'NONE',  ( 2.499999999999998668, -4.916402349214439305, -20.41639017900864772 ) ) ;
#8392 = CIRCLE ( 'NONE', #11374, 5.000000000000000000 ) ;
#8393 = VECTOR ( 'NONE', #974, 1000.000000000000000 ) ;
#8394 = DIRECTION ( 'NONE',  ( 1.000000000000000000, -0.000000000000000000, -0.000000000000000000 ) ) ;
#8395 = DIRECTION ( 'NONE',  ( 1.000000000000000000, 0.000000000000000000, 0.000000000000000000 ) ) ;
#8396 = ADVANCED_FACE ( 'NONE', ( #4844 ), #1090, .F. ) ;
#8397 = ORIENTED_EDGE ( 'NONE', *, *, #1716, .F. ) ;
#8398 = EDGE_CURVE ( 'NONE', #10665, #11209, #7856, .T. ) ;
#8399 = AXIS2_PLACEMENT_3D ( 'NONE', #10062, #2421, #11908 ) ;
#8400 = CARTESIAN_POINT ( 'NONE',  ( 0.000000000000000000, 0.000000000000000000, -1.000000000000000000 ) ) ;
#8401 = CARTESIAN_POINT ( 'NONE',  ( 46.00000000000000000, -3.499999999999998668, -38.49999999999998579 ) ) ;
#8402 = VERTEX_POINT ( 'NONE', #3908 ) ;
#8403 = CARTESIAN_POINT ( 'NONE',  ( 15.00000000000000355, 44.00000000000001421, 0.000000000000000000 ) ) ;
#8404 = DIRECTION ( 'NONE',  ( -0.000000000000000000, 1.000000000000000000, 1.224646799147353207E-16 ) ) ;
#8405 = ORIENTED_EDGE ( 'NONE', *, *, #4945, .T. ) ;
#8406 = DIRECTION ( 'NONE',  ( -1.000000000000000000, -0.000000000000000000, -0.000000000000000000 ) ) ;
#8407 = UNCERTAINTY_MEASURE_WITH_UNIT (LENGTH_MEASURE( 1.000000000000000082E-05 ), #6000, 'distance_accuracy_value', 'NONE');
#8408 = ORIENTED_EDGE ( 'NONE', *, *, #9936, .F. ) ;
#8409 = AXIS2_PLACEMENT_3D ( 'NONE', #11080, #10260, #11132 ) ;
#8410 = TOROIDAL_SURFACE ( 'NONE', #8604, 4.000000000000000000, 0.2500000000000000000 ) ;
#8411 =( REPRESENTATION_RELATIONSHIP ('NONE','NONE', #9709, #5877 ) REPRESENTATION_RELATIONSHIP_WITH_TRANSFORMATION ( #1335 )SHAPE_REPRESENTATION_RELATIONSHIP( ) );
#8412 = CARTESIAN_POINT ( 'NONE',  ( 4.999999999999999112, 0.000000000000000000, 0.000000000000000000 ) ) ;
#8413 = CARTESIAN_POINT ( 'NONE',  ( 0.000000000000000000, 0.000000000000000000, 0.000000000000000000 ) ) ;
#8414 = ADVANCED_FACE ( 'NONE', ( #4903 ), #2907, .F. ) ;
#8415 = DIRECTION ( 'NONE',  ( 0.000000000000000000, 0.000000000000000000, 1.000000000000000000 ) ) ;
#8416 = CARTESIAN_POINT ( 'NONE',  ( -20.63749999999999929, 0.000000000000000000, 0.000000000000000000 ) ) ;
#8417 = VECTOR ( 'NONE', #7655, 1000.000000000000000 ) ;
#8418 = VECTOR ( 'NONE', #4654, 1000.000000000000000 ) ;
#8419 = EDGE_LOOP ( 'NONE', ( #9407, #10354, #11539, #624 ) ) ;
#8420 = ORIENTED_EDGE ( 'NONE', *, *, #1801, .F. ) ;
#8421 = AXIS2_PLACEMENT_3D ( 'NONE', #10966, #342, #5981 ) ;
#8422 = CARTESIAN_POINT ( 'NONE',  ( -36.00000000000000711, 0.000000000000000000, 0.000000000000000000 ) ) ;
#8423 = AXIS2_PLACEMENT_3D ( 'NONE', #8934, #7060, #11786 ) ;
#8424 = ORIENTED_EDGE ( 'NONE', *, *, #9544, .F. ) ;
#8425 = DIRECTION ( 'NONE',  ( -1.000000000000000000, 0.000000000000000000, 0.000000000000000000 ) ) ;
#8426 = SHAPE_REPRESENTATION ( 'handle', ( #6056 ), #7232 ) ;
#8427 = ORIENTED_EDGE ( 'NONE', *, *, #11650, .F. ) ;
#8428 = CARTESIAN_POINT ( 'NONE',  ( -1.500000000000000444, 5.750000000000000000, 0.000000000000000000 ) ) ;
#8429 = CARTESIAN_POINT ( 'NONE',  ( -1.500000000000001332, 0.000000000000000000, -6.975000000000000533 ) ) ;
#8430 = VECTOR ( 'NONE', #5677, 1000.000000000000000 ) ;
#8431 = CIRCLE ( 'NONE', #6227, 4.799999999999999822 ) ;
#8432 = VECTOR ( 'NONE', #4776, 1000.000000000000000 ) ;
#8433 = ORIENTED_EDGE ( 'NONE', *, *, #12309, .T. ) ;
#8434 = CARTESIAN_POINT ( 'NONE',  ( 0.000000000000000000, 0.000000000000000000, 20.24900000002024569 ) ) ;
#8435 = VERTEX_POINT ( 'NONE', #8664 ) ;
#8436 = CARTESIAN_POINT ( 'NONE',  ( -20.00000000000000000, 44.00000000000001421, 12.50000000000000000 ) ) ;
#8437 = ORIENTED_EDGE ( 'NONE', *, *, #8174, .T. ) ;
#8438 = AXIS2_PLACEMENT_3D ( 'NONE', #8824, #7893, #360 ) ;
#8439 = LINE ( 'NONE', #3876, #6909 ) ;
#8440 = VERTEX_POINT ( 'NONE', #11515 ) ;
#8441 = DIRECTION ( 'NONE',  ( 0.000000000000000000, 0.000000000000000000, -1.000000000000000000 ) ) ;
#8442 = ADVANCED_FACE ( 'NONE', ( #9533 ), #5850, .T. ) ;
#8443 =( GEOMETRIC_REPRESENTATION_CONTEXT ( 3 ) GLOBAL_UNCERTAINTY_ASSIGNED_CONTEXT ( ( #523 ) ) GLOBAL_UNIT_ASSIGNED_CONTEXT ( ( #3240, #2986, #8742 ) ) REPRESENTATION_CONTEXT ( 'NONE', 'WORKASPACE' ) );
#8444 = VECTOR ( 'NONE', #11886, 1000.000000000000000 ) ;
#8445 = AXIS2_PLACEMENT_3D ( 'NONE', #3303, #9981, #5297 ) ;
#8446 = CARTESIAN_POINT ( 'NONE',  ( 2.399999999999999467, 0.000000000000000000, 0.000000000000000000 ) ) ;
#8447 = EDGE_CURVE ( 'NONE', #7959, #9611, #5594, .T. ) ;
#8448 = CIRCLE ( 'NONE', #9054, 4.800000000000000711 ) ;
#8449 = CARTESIAN_POINT ( 'NONE',  ( -0.5590169943749470072, 0.000000000000000000, -5.750000000000000000 ) ) ;
#8450 = DIRECTION ( 'NONE',  ( -1.000000000000000000, -0.000000000000000000, -0.000000000000000000 ) ) ;
#8451 = VERTEX_POINT ( 'NONE', #3774 ) ;
#8452 = ORIENTED_EDGE ( 'NONE', *, *, #1497, .F. ) ;
#8453 = DIRECTION ( 'NONE',  ( 0.000000000000000000, -0.8660254037844433705, 0.4999999999999920064 ) ) ;
#8454 = CARTESIAN_POINT ( 'NONE',  ( 33.00000000000000000, 6.368163355566238354E-16, -36.79999999999999716 ) ) ;
#8455 = CIRCLE ( 'NONE', #8856, 5.000000000000004441 ) ;
#8456 = DIRECTION ( 'NONE',  ( 1.000000000000000000, 0.000000000000000000, 0.000000000000000000 ) ) ;
#8457 = CIRCLE ( 'NONE', #75, 9.600000000009600853 ) ;
#8458 = ORIENTED_EDGE ( 'NONE', *, *, #6933, .T. ) ;
#8459 = DIRECTION ( 'NONE',  ( 0.000000000000000000, 1.000000000000000000, -1.224646799147353207E-16 ) ) ;
#8460 = EDGE_CURVE ( 'NONE', #3361, #11522, #11776, .T. ) ;
#8461 = ADVANCED_FACE ( 'NONE', ( #3960 ), #5774, .T. ) ;
#8462 = ADVANCED_FACE ( 'NONE', ( #11575 ), #1025, .T. ) ;
#8463 = ADVANCED_FACE ( 'NONE', ( #7594 ), #7724, .T. ) ;
#8464 =( NAMED_UNIT ( * ) PLANE_ANGLE_UNIT ( ) SI_UNIT ( $, .RADIAN. ) );
#8465 = DIRECTION ( 'NONE',  ( -0.000000000000000000, -0.7051068025914619675, -0.7091011189803928527 ) ) ;
#8466 = CIRCLE ( 'NONE', #8663, 5.000000000000004441 ) ;
#8467 = ORIENTED_EDGE ( 'NONE', *, *, #2387, .F. ) ;
#8468 = CARTESIAN_POINT ( 'NONE',  ( -2.000000000000000000, -6.429618962271402616, -1.000000000000000000 ) ) ;
#8469 = CARTESIAN_POINT ( 'NONE',  ( 4.999999999999999112, 20.41639017900859088, 4.916402349214653356 ) ) ;
#8470 = VERTEX_POINT ( 'NONE', #6784 ) ;
#8471 = DIRECTION ( 'NONE',  ( 0.000000000000000000, 0.000000000000000000, 1.000000000000000000 ) ) ;
#8472 = LINE ( 'NONE', #12128, #1824 ) ;
#8473 = VERTEX_POINT ( 'NONE', #10585 ) ;
#8474 = CARTESIAN_POINT ( 'NONE',  ( 26.00000000000000355, 0.000000000000000000, -41.99999999999999289 ) ) ;
#8475 = VERTEX_POINT ( 'NONE', #2844 ) ;
#8476 = AXIS2_PLACEMENT_3D ( 'NONE', #10668, #1037, #11467 ) ;
#8477 = LINE ( 'NONE', #900, #11565 ) ;
#8478 = EDGE_CURVE ( 'NONE', #4680, #9643, #2029, .T. ) ;
#8479 = CARTESIAN_POINT ( 'NONE',  ( 5.200000000000002842, 3.061616997868383634E-16, -2.500000000000000444 ) ) ;
#8480 = DIRECTION ( 'NONE',  ( 0.000000000000000000, 0.000000000000000000, -1.000000000000000000 ) ) ;
#8481 = CARTESIAN_POINT ( 'NONE',  ( 20.00000000000000000, 40.00000000000001421, -12.50000000000000000 ) ) ;
#8482 = FACE_OUTER_BOUND ( 'NONE', #12048, .T. ) ;
#8483 = ORIENTED_EDGE ( 'NONE', *, *, #10580, .T. ) ;
#8484 = VERTEX_POINT ( 'NONE', #9725 ) ;
#8485 = FACE_OUTER_BOUND ( 'NONE', #5525, .T. ) ;
#8486 = ORIENTED_EDGE ( 'NONE', *, *, #10306, .T. ) ;
#8487 = PRODUCT_CONTEXT ( 'NONE', #2171, 'mechanical' ) ;
#8488 = ORIENTED_EDGE ( 'NONE', *, *, #1102, .F. ) ;
#8489 = CARTESIAN_POINT ( 'NONE',  ( 42.00000000000000000, 1.908195823574506293E-17, -41.99999999999998579 ) ) ;
#8490 = EDGE_CURVE ( 'NONE', #1270, #2996, #8600, .T. ) ;
#8491 = ADVANCED_FACE ( 'NONE', ( #3155 ), #275, .T. ) ;
#8492 = AXIS2_PLACEMENT_3D ( 'NONE', #4638, #2748, #7711 ) ;
#8493 = MANIFOLD_SOLID_BREP ( 'Keyway', #10359 ) ;
#8494 = ORIENTED_EDGE ( 'NONE', *, *, #4270, .F. ) ;
#8495 = ORIENTED_EDGE ( 'NONE', *, *, #6981, .T. ) ;
#8496 = DIRECTION ( 'NONE',  ( 1.000000000000000000, -0.000000000000000000, -0.000000000000000000 ) ) ;
#8497 = CARTESIAN_POINT ( 'NONE',  ( 4.999999999999999112, 0.000000000000000000, 0.000000000000000000 ) ) ;
#8498 = DIRECTION ( 'NONE',  ( -1.000000000000000000, 0.000000000000000000, -0.000000000000000000 ) ) ;
#8499 = EDGE_LOOP ( 'NONE', ( #7118, #5947, #4835, #6358 ) ) ;
#8500 = DIRECTION ( 'NONE',  ( -1.000000000000000000, 0.000000000000000000, 0.000000000000000000 ) ) ;
#8501 = ORIENTED_EDGE ( 'NONE', *, *, #9636, .F. ) ;
#8502 = AXIS2_PLACEMENT_3D ( 'NONE', #8187, #6315, #3316 ) ;
#8503 =( NAMED_UNIT ( * ) PLANE_ANGLE_UNIT ( ) SI_UNIT ( $, .RADIAN. ) );
#8504 = CARTESIAN_POINT ( 'NONE',  ( 1.600000000000000089, 8.572527594031473190E-16, -7.000000000000000000 ) ) ;
#8505 = ORIENTED_EDGE ( 'NONE', *, *, #11233, .T. ) ;
#8506 = CARTESIAN_POINT ( 'NONE',  ( 0.000000000000000000, 0.5192545390863916310, 0.000000000000000000 ) ) ;
#8507 = DIRECTION ( 'NONE',  ( 0.000000000000000000, 0.000000000000000000, 1.000000000000000000 ) ) ;
#8508 = CARTESIAN_POINT ( 'NONE',  ( 26.00000000000000355, 0.000000000000000000, 0.000000000000000000 ) ) ;
#8509 = CARTESIAN_POINT ( 'NONE',  ( 0.000000000000000000, 0.000000000000000000, 0.000000000000000000 ) ) ;
#8510 = VERTEX_POINT ( 'NONE', #10770 ) ;
#8511 = ORIENTED_EDGE ( 'NONE', *, *, #1570, .T. ) ;
#8512 = DIRECTION ( 'NONE',  ( -1.000000000000000000, 0.000000000000000000, 0.000000000000000000 ) ) ;
#8513 =( LENGTH_UNIT ( ) NAMED_UNIT ( * ) SI_UNIT ( .MILLI., .METRE. ) );
#8514 = DIRECTION ( 'NONE',  ( -1.000000000000000000, -0.000000000000000000, -0.000000000000000000 ) ) ;
#8515 = CYLINDRICAL_SURFACE ( 'NONE', #5899, 20.24900000002024569 ) ;
#8516 = ADVANCED_FACE ( 'NONE', ( #2205 ), #5140, .T. ) ;
#8517 = EDGE_LOOP ( 'NONE', ( #8732, #1605 ) ) ;
#8518 = LINE ( 'NONE', #131, #6385 ) ;
#8519 = CARTESIAN_POINT ( 'NONE',  ( 4.999999999999999112, 19.60720892790252989, 11.14352537685181588 ) ) ;
#8520 = DIRECTION ( 'NONE',  ( -1.000000000000000000, 0.000000000000000000, -0.000000000000000000 ) ) ;
#8521 = CARTESIAN_POINT ( 'NONE',  ( 4.999999999999999112, 20.41639017900859088, -4.916402349214653356 ) ) ;
#8522 = DIRECTION ( 'NONE',  ( 0.000000000000000000, 0.000000000000000000, -1.000000000000000000 ) ) ;
#8523 = ORIENTED_EDGE ( 'NONE', *, *, #7992, .F. ) ;
#8524 = ADVANCED_FACE ( 'NONE', ( #9038 ), #4323, .T. ) ;
#8525 = DIRECTION ( 'NONE',  ( 0.000000000000000000, -0.7071067811865389130, -0.7071067811865561215 ) ) ;
#8526 = DIRECTION ( 'NONE',  ( 0.000000000000000000, 0.8660254037844363761, 0.5000000000000041078 ) ) ;
#8527 = ORIENTED_EDGE ( 'NONE', *, *, #8367, .F. ) ;
#8528 = DIRECTION ( 'NONE',  ( 0.000000000000000000, 0.000000000000000000, 1.000000000000000000 ) ) ;
#8529 = UNCERTAINTY_MEASURE_WITH_UNIT (LENGTH_MEASURE( 1.000000000000000082E-05 ), #1548, 'distance_accuracy_value', 'NONE');
#8530 = EDGE_CURVE ( 'NONE', #536, #11283, #7964, .T. ) ;
#8531 = MANIFOLD_SOLID_BREP ( 'Hex', #8184 ) ;
#8532 = EDGE_LOOP ( 'NONE', ( #10164, #2135, #4310, #5971 ) ) ;
#8533 = EDGE_CURVE ( 'NONE', #9327, #10227, #5023, .T. ) ;
#8534 = SURFACE_SIDE_STYLE ('',( #17 ) ) ;
#8535 = LINE ( 'NONE', #10466, #10591 ) ;
#8536 = PLANE ( 'NONE',  #8020 ) ;
#8537 = CARTESIAN_POINT ( 'NONE',  ( 4.999999999999999112, 5.622796541391749336, -13.09267581720861173 ) ) ;
#8538 = DIRECTION ( 'NONE',  ( 0.000000000000000000, 0.000000000000000000, -1.000000000000000000 ) ) ;
#8539 = ORIENTED_EDGE ( 'NONE', *, *, #9635, .F. ) ;
#8540 = ORIENTED_EDGE ( 'NONE', *, *, #1462, .T. ) ;
#8541 = DIRECTION ( 'NONE',  ( 0.000000000000000000, 0.000000000000000000, 1.000000000000000000 ) ) ;
#8542 = EDGE_LOOP ( 'NONE', ( #5145, #4742 ) ) ;
#8543 = DIRECTION ( 'NONE',  ( 0.000000000000000000, 0.000000000000000000, -1.000000000000000000 ) ) ;
#8544 = ADVANCED_FACE ( 'NONE', ( #8103 ), #7911, .T. ) ;
#8545 = APPLICATION_PROTOCOL_DEFINITION ( 'draft international standard', 'automotive_design', 1998, #3702 ) ;
#8546 = ORIENTED_EDGE ( 'NONE', *, *, #9103, .F. ) ;
#8547 = EDGE_CURVE ( 'NONE', #9803, #1217, #599, .T. ) ;
#8548 = FACE_OUTER_BOUND ( 'NONE', #5722, .T. ) ;
#8549 = DIRECTION ( 'NONE',  ( -1.000000000000000000, 0.000000000000000000, -0.000000000000000000 ) ) ;
#8550 = ORIENTED_EDGE ( 'NONE', *, *, #3332, .T. ) ;
#8551 = ORIENTED_EDGE ( 'NONE', *, *, #3267, .F. ) ;
#8552 = DIRECTION ( 'NONE',  ( 1.000000000000000000, 0.000000000000000000, 0.000000000000000000 ) ) ;
#8553 = DIRECTION ( 'NONE',  ( 0.000000000000000000, -0.5446390350150287496, 0.8386705679454229401 ) ) ;
#8554 = DIRECTION ( 'NONE',  ( 0.000000000000000000, 0.000000000000000000, -1.000000000000000000 ) ) ;
#8555 = EDGE_LOOP ( 'NONE', ( #10730, #2149, #7879, #2855, #8204 ) ) ;
#8556 = ADVANCED_FACE ( 'NONE', ( #9152, #12120 ), #9280, .F. ) ;
#8557 = EDGE_CURVE ( 'NONE', #6059, #11661, #10184, .T. ) ;
#8558 = FACE_OUTER_BOUND ( 'NONE', #5329, .T. ) ;
#8559 = VERTEX_POINT ( 'NONE', #9335 ) ;
#8560 = VERTEX_POINT ( 'NONE', #2637 ) ;
#8561 = CARTESIAN_POINT ( 'NONE',  ( 0.000000000000000000, 15.57980286237503442, -22.05152472667113983 ) ) ;
#8562 = EDGE_LOOP ( 'NONE', ( #308, #2727, #9525, #2622 ) ) ;
#8563 = CARTESIAN_POINT ( 'NONE',  ( 2.499999999999999556, -15.22291137398912397, -14.46592441914980753 ) ) ;
#8564 = VECTOR ( 'NONE', #4141, 1000.000000000000000 ) ;
#8565 = DIRECTION ( 'NONE',  ( 0.000000000000000000, 0.3826834323650841196, 0.9238795325112890700 ) ) ;
#8566 = CIRCLE ( 'NONE', #5569, 9.600000000009600853 ) ;
#8567 = CARTESIAN_POINT ( 'NONE',  ( 2.499999999999999556, -15.57980286237457435, -22.05152472667146668 ) ) ;
#8568 = DIRECTION ( 'NONE',  ( -1.000000000000000000, -3.903127820947815962E-18, 0.000000000000000000 ) ) ;
#8569 = ORIENTED_EDGE ( 'NONE', *, *, #10971, .T. ) ;
#8570 = VERTEX_POINT ( 'NONE', #3576 ) ;
#8571 = CARTESIAN_POINT ( 'NONE',  ( 4.999999999999999112, -18.05452603534171985, 9.168210874537514599 ) ) ;
#8572 = FILL_AREA_STYLE ('',( #3819 ) ) ;
#8573 = CARTESIAN_POINT ( 'NONE',  ( 46.00000000000000000, -3.545505594901965818, -38.47446598704267728 ) ) ;
#8574 = DIRECTION ( 'NONE',  ( 0.9961946980917455452, 1.067350013832296744E-17, 0.08715574274765813811 ) ) ;
#8575 = ORIENTED_EDGE ( 'NONE', *, *, #2538, .F. ) ;
#8576 = LINE ( 'NONE', #6762, #635 ) ;
#8577 =( REPRESENTATION_RELATIONSHIP ('NONE','NONE', #9709, #11292 ) REPRESENTATION_RELATIONSHIP_WITH_TRANSFORMATION ( #9676 )SHAPE_REPRESENTATION_RELATIONSHIP( ) );
#8578 = AXIS2_PLACEMENT_3D ( 'NONE', #9500, #923, #5804 ) ;
#8579 = CYLINDRICAL_SURFACE ( 'NONE', #7011, 27.00000000002699707 ) ;
#8580 = LINE ( 'NONE', #3705, #2307 ) ;
#8581 = DIRECTION ( 'NONE',  ( 1.000000000000000000, 0.000000000000000000, 0.000000000000000000 ) ) ;
#8582 = DIRECTION ( 'NONE',  ( 1.000000000000000000, -0.000000000000000000, 0.000000000000000000 ) ) ;
#8583 = AXIS2_PLACEMENT_3D ( 'NONE', #5905, #5079, #1137 ) ;
#8584 = AXIS2_PLACEMENT_3D ( 'NONE', #10878, #8949, #9828 ) ;
#8585 = ORIENTED_EDGE ( 'NONE', *, *, #5253, .F. ) ;
#8586 = DIRECTION ( 'NONE',  ( 0.000000000000000000, 0.000000000000000000, -1.000000000000000000 ) ) ;
#8587 = FACE_OUTER_BOUND ( 'NONE', #933, .T. ) ;
#8588 = EDGE_LOOP ( 'NONE', ( #1136, #12001 ) ) ;
#8589 = CYLINDRICAL_SURFACE ( 'NONE', #7696, 7.000000000000000000 ) ;
#8590 = VERTEX_POINT ( 'NONE', #5570 ) ;
#8591 = VECTOR ( 'NONE', #1714, 1000.000000000000000 ) ;
#8592 = EDGE_CURVE ( 'NONE', #7124, #1873, #10000, .T. ) ;
#8593 = CARTESIAN_POINT ( 'NONE',  ( 4.999999999999999112, 0.000000000000000000, 0.000000000000000000 ) ) ;
#8594 = DIRECTION ( 'NONE',  ( 1.000000000000000000, 0.000000000000000000, 0.000000000000000000 ) ) ;
#8595 = EDGE_CURVE ( 'NONE', #4367, #2664, #5332, .T. ) ;
#8596 = DIRECTION ( 'NONE',  ( 1.000000000000000000, 0.000000000000000000, 0.000000000000000000 ) ) ;
#8597 = LINE ( 'NONE', #3722, #28 ) ;
#8598 = ORIENTED_EDGE ( 'NONE', *, *, #3489, .T. ) ;
#8599 = ORIENTED_EDGE ( 'NONE', *, *, #296, .T. ) ;
#8600 = CIRCLE ( 'NONE', #6405, 5.000000000000000000 ) ;
#8601 = VERTEX_POINT ( 'NONE', #7396 ) ;
#8602 = DIRECTION ( 'NONE',  ( 0.000000000000000000, 0.000000000000000000, -1.000000000000000000 ) ) ;
#8603 = APPLICATION_PROTOCOL_DEFINITION ( 'draft international standard', 'automotive_design', 1998, #18 ) ;
#8604 = AXIS2_PLACEMENT_3D ( 'NONE', #4891, #12187, #3645 ) ;
#8605 = ORIENTED_EDGE ( 'NONE', *, *, #579, .T. ) ;
#8606 = DIRECTION ( 'NONE',  ( -1.000000000000000000, -0.000000000000000000, -0.000000000000000000 ) ) ;
#8607 = VERTEX_POINT ( 'NONE', #10317 ) ;
#8608 = CIRCLE ( 'NONE', #2807, 5.000000000000000000 ) ;
#8609 = VERTEX_POINT ( 'NONE', #2511 ) ;
#8610 = CARTESIAN_POINT ( 'NONE',  ( 37.00000000000000711, -2.172883482918394282, 4.280020720704565740 ) ) ;
#8611 = CARTESIAN_POINT ( 'NONE',  ( -36.00000000000000711, -4.898587196589413815E-15, -40.00000000000000711 ) ) ;
#8612 = EDGE_CURVE ( 'NONE', #978, #7155, #10091, .T. ) ;
#8613 = AXIS2_PLACEMENT_3D ( 'NONE', #2588, #10224, #10333 ) ;
#8614 = EDGE_CURVE ( 'NONE', #7019, #1992, #6517, .T. ) ;
#8615 = AXIS2_PLACEMENT_3D ( 'NONE', #11713, #9975, #8801 ) ;
#8616 = DIRECTION ( 'NONE',  ( -1.000000000000000000, 0.000000000000000000, 0.000000000000000000 ) ) ;
#8618 = EDGE_CURVE ( 'NONE', #8041, #8258, #11198, .T. ) ;
#8617 = CARTESIAN_POINT ( 'NONE',  ( 36.00000000000000711, 0.000000000000000000, -7.500000000000000888 ) ) ;
#8619 = EDGE_LOOP ( 'NONE', ( #9559, #7006, #5769, #10464 ) ) ;
#8620 = CARTESIAN_POINT ( 'NONE',  ( -38.00000000000000000, 0.000000000000000000, -5.999999999999999112 ) ) ;
#8621 = EDGE_LOOP ( 'NONE', ( #2902, #4377, #2162, #6733 ) ) ;
#8622 = ORIENTED_EDGE ( 'NONE', *, *, #5424, .F. ) ;
#8623 =( GEOMETRIC_REPRESENTATION_CONTEXT ( 3 ) GLOBAL_UNCERTAINTY_ASSIGNED_CONTEXT ( ( #3658 ) ) GLOBAL_UNIT_ASSIGNED_CONTEXT ( ( #4312, #1452, #1510 ) ) REPRESENTATION_CONTEXT ( 'NONE', 'WORKASPACE' ) );
#8624 = CIRCLE ( 'NONE', #3422, 5.199999999999996625 ) ;
#8625 = CARTESIAN_POINT ( 'NONE',  ( -20.00000000000000000, 44.00000000000001421, -12.50000000000000000 ) ) ;
#8626 = AXIS2_PLACEMENT_3D ( 'NONE', #2953, #11452, #10707 ) ;
#8627 = AXIS2_PLACEMENT_3D ( 'NONE', #12210, #6534, #6349 ) ;
#8628 = ORIENTED_EDGE ( 'NONE', *, *, #4658, .F. ) ;
#8629 = DIRECTION ( 'NONE',  ( 0.000000000000000000, -0.000000000000000000, 1.000000000000000000 ) ) ;
#8630 = VECTOR ( 'NONE', #12040, 1000.000000000000000 ) ;
#8631 = EDGE_CURVE ( 'NONE', #4672, #4056, #6333, .T. ) ;
#8632 = LINE ( 'NONE', #118, #5407 ) ;
#8633 = VECTOR ( 'NONE', #12272, 1000.000000000000000 ) ;
#8634 = AXIS2_PLACEMENT_3D ( 'NONE', #10255, #626, #1751 ) ;
#8635 = AXIS2_PLACEMENT_3D ( 'NONE', #4893, #3950, #3015 ) ;
#8636 = AXIS2_PLACEMENT_3D ( 'NONE', #7853, #2322, #7146 ) ;
#8637 = DIRECTION ( 'NONE',  ( 0.000000000000000000, 0.000000000000000000, -1.000000000000000000 ) ) ;
#8638 = DIRECTION ( 'NONE',  ( -0.5000000000000051070, 1.060575238724903217E-16, -0.8660254037844355990 ) ) ;
#8639 = VERTEX_POINT ( 'NONE', #6394 ) ;
#8640 = CARTESIAN_POINT ( 'NONE',  ( 4.999999999999999112, 14.40062958310465469, 8.872489362018239234 ) ) ;
#8641 = DIRECTION ( 'NONE',  ( 1.000000000000000000, -0.000000000000000000, -0.000000000000000000 ) ) ;
#8642 = DIRECTION ( 'NONE',  ( 0.000000000000000000, -1.000000000000000000, -0.000000000000000000 ) ) ;
#8643 = ORIENTED_EDGE ( 'NONE', *, *, #8979, .T. ) ;
#8644 = PLANE ( 'NONE',  #6582 ) ;
#8645 = CIRCLE ( 'NONE', #5638, 14.24900000001425227 ) ;
#8646 = VECTOR ( 'NONE', #8120, 1000.000000000000000 ) ;
#8647 = EDGE_CURVE ( 'NONE', #1819, #11306, #4571, .T. ) ;
#8648 = AXIS2_PLACEMENT_3D ( 'NONE', #12299, #3692, #10308 ) ;
#8649 = LINE ( 'NONE', #10453, #6206 ) ;
#8650 = CARTESIAN_POINT ( 'NONE',  ( 0.000000000000000000, 0.000000000000000000, 12.50000000000000000 ) ) ;
#8651 = CARTESIAN_POINT ( 'NONE',  ( -20.63749999999999929, 0.000000000000000000, 0.000000000000000000 ) ) ;
#8652 = DIRECTION ( 'NONE',  ( 0.000000000000000000, -0.000000000000000000, -1.000000000000000000 ) ) ;
#8653 = AXIS2_PLACEMENT_3D ( 'NONE', #8651, #2828, #8710 ) ;
#8654 = VERTEX_POINT ( 'NONE', #9215 ) ;
#8655 = DIRECTION ( 'NONE',  ( -1.000000000000000000, 0.000000000000000000, 0.000000000000000000 ) ) ;
#8656 = CIRCLE ( 'NONE', #4250, 21.00000000002100009 ) ;
#8657 = DIRECTION ( 'NONE',  ( 0.000000000000000000, -0.8660254037844328234, -0.5000000000000101030 ) ) ;
#8658 = VERTEX_POINT ( 'NONE', #12007 ) ;
#8659 = CARTESIAN_POINT ( 'NONE',  ( 50.00005079999999680, 0.000000000000000000, 0.000000000000000000 ) ) ;
#8660 = UNCERTAINTY_MEASURE_WITH_UNIT (LENGTH_MEASURE( 1.000000000000000082E-05 ), #8708, 'distance_accuracy_value', 'NONE');
#8661 = MANIFOLD_SOLID_BREP ( 'Keyway', #177 ) ;
#8662 = ORIENTED_EDGE ( 'NONE', *, *, #2118, .T. ) ;
#8663 = AXIS2_PLACEMENT_3D ( 'NONE', #3604, #8425, #7424 ) ;
#8664 = CARTESIAN_POINT ( 'NONE',  ( 4.999999999999999112, -16.90755573046745752, 6.716513609244448624 ) ) ;
#8665 = DIRECTION ( 'NONE',  ( 0.000000000000000000, 0.000000000000000000, -1.000000000000000000 ) ) ;
#8666 = CARTESIAN_POINT ( 'NONE',  ( 0.000000000000000000, 0.5192545390863916310, -1.000000000000000000 ) ) ;
#8667 = CARTESIAN_POINT ( 'NONE',  ( -2.354826896168714434, -6.962563485461402024, 0.000000000000000000 ) ) ;
#8668 = VERTEX_POINT ( 'NONE', #3520 ) ;
#8669 = EDGE_LOOP ( 'NONE', ( #10834, #12332, #8908, #983 ) ) ;
#8670 = FACE_OUTER_BOUND ( 'NONE', #4545, .T. ) ;
#8671 = EDGE_LOOP ( 'NONE', ( #7374, #7202, #6248, #5783 ) ) ;
#8672 = CARTESIAN_POINT ( 'NONE',  ( 36.00000000000000711, -12.50000000000000000, -24.50000000000000000 ) ) ;
#8673 = ADVANCED_FACE ( 'NONE', ( #7339 ), #11017, .T. ) ;
#8674 = APPLICATION_PROTOCOL_DEFINITION ( 'draft international standard', 'automotive_design', 1998, #11984 ) ;
#8675 = COLOUR_RGB ( '',0.8941176470588234615, 0.8941176470588234615, 0.8941176470588234615 ) ;
#8676 = VERTEX_POINT ( 'NONE', #3704 ) ;
#8677 = EDGE_CURVE ( 'NONE', #6998, #9896, #11499, .T. ) ;
#8678 = ORIENTED_EDGE ( 'NONE', *, *, #4239, .F. ) ;
#8679 = ORIENTED_EDGE ( 'NONE', *, *, #9369, .F. ) ;
#8680 = CARTESIAN_POINT ( 'NONE',  ( 36.00000000000000711, 0.000000000000000000, -41.99999999999999289 ) ) ;
#8681 = CARTESIAN_POINT ( 'NONE',  ( 2.354826896168714434, -6.962563485461402024, -1.000000000000000000 ) ) ;
#8682 = MECHANICAL_DESIGN_GEOMETRIC_PRESENTATION_REPRESENTATION (  '', ( #6278 ), #1887 ) ;
#8683 = DIRECTION ( 'NONE',  ( -1.000000000000000000, -0.000000000000000000, -0.000000000000000000 ) ) ;
#8684 = CARTESIAN_POINT ( 'NONE',  ( 4.999999999999999112, 0.000000000000000000, 0.000000000000000000 ) ) ;
#8685 = ORIENTED_EDGE ( 'NONE', *, *, #8913, .F. ) ;
#8686 = FACE_BOUND ( 'NONE', #1539, .T. ) ;
#8687 = ORIENTED_EDGE ( 'NONE', *, *, #10071, .T. ) ;
#8688 = EDGE_CURVE ( 'NONE', #5429, #702, #8608, .T. ) ;
#8689 = ORIENTED_EDGE ( 'NONE', *, *, #87, .F. ) ;
#8690 = CYLINDRICAL_SURFACE ( 'NONE', #1422, 4.799999999999998934 ) ;
#8691 = EDGE_CURVE ( 'NONE', #649, #1430, #6414, .T. ) ;
#8692 = AXIS2_PLACEMENT_3D ( 'NONE', #8474, #6588, #2836 ) ;
#8693 = VERTEX_POINT ( 'NONE', #12307 ) ;
#8694 = DIRECTION ( 'NONE',  ( -1.000000000000000000, 0.000000000000000000, 0.000000000000000000 ) ) ;
#8695 = EDGE_CURVE ( 'NONE', #4331, #5656, #8015, .T. ) ;
#8696 = CARTESIAN_POINT ( 'NONE',  ( 5.000000000000000000, 0.000000000000000000, -1.500000000000000000 ) ) ;
#8697 = ORIENTED_EDGE ( 'NONE', *, *, #9102, .T. ) ;
#8698 = VECTOR ( 'NONE', #129, 1000.000000000000000 ) ;
#8699 = DIRECTION ( 'NONE',  ( -1.000000000000000000, 0.000000000000000000, -0.000000000000000000 ) ) ;
#8700 = CARTESIAN_POINT ( 'NONE',  ( 43.00000000000000000, -2.824006678639516377, 3.881363971466655904 ) ) ;
#8701 = VERTEX_POINT ( 'NONE', #8764 ) ;
#8702 = DIRECTION ( 'NONE',  ( 0.000000000000000000, 0.000000000000000000, 1.000000000000000000 ) ) ;
#8703 = CARTESIAN_POINT ( 'NONE',  ( 43.00000000000000000, 3.903127820947864496E-18, 0.000000000000000000 ) ) ;
#8704 = DIRECTION ( 'NONE',  ( 1.000000000000000000, 0.000000000000000000, -0.000000000000000000 ) ) ;
#8705 = ORIENTED_EDGE ( 'NONE', *, *, #1116, .T. ) ;
#8706 = CARTESIAN_POINT ( 'NONE',  ( 0.000000000000000000, -5.622796541391657854, 13.09267581720864904 ) ) ;
#8707 = PRODUCT_DEFINITION ( 'UNKNOWN', '', #10434, #2269 ) ;
#8708 =( LENGTH_UNIT ( ) NAMED_UNIT ( * ) SI_UNIT ( .MILLI., .METRE. ) );
#8709 = LINE ( 'NONE', #2079, #6207 ) ;
#8710 = DIRECTION ( 'NONE',  ( 0.000000000000000000, 0.000000000000000000, -1.000000000000000000 ) ) ;
#8711 = DIRECTION ( 'NONE',  ( 1.000000000000000000, 0.000000000000000000, 0.000000000000000000 ) ) ;
#8712 = ORIENTED_EDGE ( 'NONE', *, *, #5544, .T. ) ;
#8713 = CARTESIAN_POINT ( 'NONE',  ( 36.00000000000000711, 0.000000000000000000, 0.000000000000000000 ) ) ;
#8714 = EDGE_CURVE ( 'NONE', #6154, #8609, #1007, .T. ) ;
#8715 = CARTESIAN_POINT ( 'NONE',  ( 36.00000000000000711, 1.456773409934505593E-31, -41.99999999999998579 ) ) ;
#8716 = EDGE_CURVE ( 'NONE', #2426, #6862, #9652, .T. ) ;
#8717 = EDGE_LOOP ( 'NONE', ( #5577, #11851, #5481, #11332 ) ) ;
#8718 = CARTESIAN_POINT ( 'NONE',  ( -20.00000000000000000, 40.00000000000000711, -12.50000000000000000 ) ) ;
#8719 = ORIENTED_EDGE ( 'NONE', *, *, #11568, .F. ) ;
#8720 = DIRECTION ( 'NONE',  ( 0.000000000000000000, 0.000000000000000000, 1.000000000000000000 ) ) ;
#8721 = CYLINDRICAL_SURFACE ( 'NONE', #5557, 4.799999999999999822 ) ;
#8722 = DIRECTION ( 'NONE',  ( 1.000000000000000000, 0.000000000000000000, 0.000000000000000000 ) ) ;
#8723 = DIRECTION ( 'NONE',  ( 0.000000000000000000, 0.000000000000000000, 1.000000000000000000 ) ) ;
#8724 = PRODUCT_DEFINITION_SHAPE ( 'NONE', 'NONE',  #11668 ) ;
#8725 = ORIENTED_EDGE ( 'NONE', *, *, #4901, .T. ) ;
#8726 = ORIENTED_EDGE ( 'NONE', *, *, #7797, .T. ) ;
#8727 = PLANE ( 'NONE',  #615 ) ;
#8728 = ORIENTED_EDGE ( 'NONE', *, *, #1119, .T. ) ;
#8729 = SURFACE_STYLE_FILL_AREA ( #4911 ) ;
#8730 = CONTEXT_DEPENDENT_SHAPE_REPRESENTATION ( #3467, #8935 ) ;
#8731 = ORIENTED_EDGE ( 'NONE', *, *, #6811, .T. ) ;
#8732 = ORIENTED_EDGE ( 'NONE', *, *, #5315, .T. ) ;
#8733 = EDGE_LOOP ( 'NONE', ( #1547, #5308, #4160, #5825 ) ) ;
#8734 = DIRECTION ( 'NONE',  ( 0.000000000000000000, 0.000000000000000000, 1.000000000000000000 ) ) ;
#8735 = DIRECTION ( 'NONE',  ( 0.1305261922200524338, 0.9914448613738102711, 0.000000000000000000 ) ) ;
#8736 = DIRECTION ( 'NONE',  ( 1.000000000000000000, -0.000000000000000000, 0.000000000000000000 ) ) ;
#8737 = DIRECTION ( 'NONE',  ( -0.7071067811865369146, 0.000000000000000000, 0.7071067811865582309 ) ) ;
#8738 = EDGE_CURVE ( 'NONE', #9966, #1854, #11788, .T. ) ;
#8739 = ORIENTED_EDGE ( 'NONE', *, *, #10535, .T. ) ;
#8740 = CARTESIAN_POINT ( 'NONE',  ( 4.999999999999999112, 0.000000000000000000, 0.000000000000000000 ) ) ;
#8741 = ORIENTED_EDGE ( 'NONE', *, *, #9926, .F. ) ;
#8742 =( NAMED_UNIT ( * ) SI_UNIT ( $, .STERADIAN. ) SOLID_ANGLE_UNIT ( ) );
#8743 = ORIENTED_EDGE ( 'NONE', *, *, #4489, .F. ) ;
#8744 = CARTESIAN_POINT ( 'NONE',  ( -10.00000000000000000, 44.00000000000001421, -12.50000000000000000 ) ) ;
#8745 = ORIENTED_EDGE ( 'NONE', *, *, #8618, .T. ) ;
#8746 = CARTESIAN_POINT ( 'NONE',  ( 4.999999999999999112, 21.74405275335758247, 5.984728032765037398 ) ) ;
#8747 = DIRECTION ( 'NONE',  ( -1.000000000000000000, 0.000000000000000000, 0.000000000000000000 ) ) ;
#8748 = EDGE_CURVE ( 'NONE', #3862, #4747, #8649, .T. ) ;
#8749 = ADVANCED_FACE ( 'NONE', ( #5703 ), #8579, .T. ) ;
#8750 = VERTEX_POINT ( 'NONE', #5832 ) ;
#8751 = MANIFOLD_SOLID_BREP ( 'M4 Clearance Hole1', #8781 ) ;
#8752 = DIRECTION ( 'NONE',  ( 1.000000000000000000, 0.000000000000000000, -0.000000000000000000 ) ) ;
#8753 = DIRECTION ( 'NONE',  ( -0.000000000000000000, -0.000000000000000000, 1.000000000000000000 ) ) ;
#8754 = EDGE_CURVE ( 'NONE', #7347, #6441, #415, .T. ) ;
#8755 = ORIENTED_EDGE ( 'NONE', *, *, #3142, .T. ) ;
#8756 = SURFACE_SIDE_STYLE ('',( #3135 ) ) ;
#8757 = DIRECTION ( 'NONE',  ( 0.000000000000000000, 0.000000000000000000, -1.000000000000000000 ) ) ;
#8758 = PLANE ( 'NONE',  #3499 ) ;
#8759 = ORIENTED_EDGE ( 'NONE', *, *, #7258, .F. ) ;
#8760 = LINE ( 'NONE', #5123, #5791 ) ;
#8761 = AXIS2_PLACEMENT_3D ( 'NONE', #8506, #1996, #4686 ) ;
#8762 = VECTOR ( 'NONE', #8752, 1000.000000000000000 ) ;
#8763 = AXIS2_PLACEMENT_3D ( 'NONE', #8966, #11701, #10771 ) ;
#8764 = CARTESIAN_POINT ( 'NONE',  ( 76.00000000000000000, 46.00000000000001421, -37.99999999999999289 ) ) ;
#8765 = DIRECTION ( 'NONE',  ( 0.000000000000000000, 0.000000000000000000, 1.000000000000000000 ) ) ;
#8766 = ADVANCED_FACE ( 'NONE', ( #6839 ), #3830, .T. ) ;
#8767 = EDGE_CURVE ( 'NONE', #2800, #11007, #2751, .T. ) ;
#8768 = DIRECTION ( 'NONE',  ( -1.000000000000000000, 0.000000000000000000, 0.000000000000000000 ) ) ;
#8769 = CARTESIAN_POINT ( 'NONE',  ( 4.999999999999999112, 1.676853263448085052, -14.14998813191267857 ) ) ;
#8770 = EDGE_CURVE ( 'NONE', #2088, #10334, #4616, .T. ) ;
#8771 = ORIENTED_EDGE ( 'NONE', *, *, #12313, .T. ) ;
#8772 = CARTESIAN_POINT ( 'NONE',  ( 4.999999999999999112, 0.000000000000000000, 0.000000000000000000 ) ) ;
#8773 = CARTESIAN_POINT ( 'NONE',  ( 4.999999999999999112, 22.83261415639502800, 14.41081992069317330 ) ) ;
#8774 = VECTOR ( 'NONE', #854, 1000.000000000000000 ) ;
#8775 = ORIENTED_EDGE ( 'NONE', *, *, #7762, .F. ) ;
#8776 = DIRECTION ( 'NONE',  ( -0.000000000000000000, 0.000000000000000000, 1.000000000000000000 ) ) ;
#8777 = AXIS2_PLACEMENT_3D ( 'NONE', #4352, #8185, #3430 ) ;
#8778 = MANIFOLD_SOLID_BREP ( 'Base-Extrude', #5987 ) ;
#8779 = ORIENTED_EDGE ( 'NONE', *, *, #11106, .F. ) ;
#8780 = CARTESIAN_POINT ( 'NONE',  ( 3.098410542199072637, -7.060458129626440815, -1.000000000000000000 ) ) ;
#8781 = CLOSED_SHELL ( 'NONE', ( #11754, #11345, #3580, #1961, #5726, #5159, #3335, #10839, #11328, #2546, #6392, #7539 ) ) ;
#8782 = EDGE_CURVE ( 'NONE', #2298, #1686, #213, .T. ) ;
#8783 = EDGE_CURVE ( 'NONE', #4084, #5720, #1259, .T. ) ;
#8784 = AXIS2_PLACEMENT_3D ( 'NONE', #3018, #4080, #7844 ) ;
#8785 = DIRECTION ( 'NONE',  ( 0.000000000000000000, 0.000000000000000000, -1.000000000000000000 ) ) ;
#8786 = DIRECTION ( 'NONE',  ( -1.000000000000000000, 0.000000000000000000, -0.000000000000000000 ) ) ;
#8787 = AXIS2_PLACEMENT_3D ( 'NONE', #9889, #6949, #10750 ) ;
#8788 = CIRCLE ( 'NONE', #4982, 9.600000000009604406 ) ;
#8789 = CARTESIAN_POINT ( 'NONE',  ( 25.00000000000000000, 0.000000000000000000, 0.000000000000000000 ) ) ;
#8790 = DIRECTION ( 'NONE',  ( -1.000000000000000000, -0.000000000000000000, -0.000000000000000000 ) ) ;
#8791 = EDGE_LOOP ( 'NONE', ( #12140, #7255, #1902, #6197 ) ) ;
#8792 = DIRECTION ( 'NONE',  ( 1.000000000000000000, 0.000000000000000000, 0.000000000000000000 ) ) ;
#8793 = ORIENTED_EDGE ( 'NONE', *, *, #3900, .F. ) ;
#8794 = CARTESIAN_POINT ( 'NONE',  ( 46.00000000000000000, 1.456773409934505593E-31, -41.99999999999998579 ) ) ;
#8795 = ORIENTED_EDGE ( 'NONE', *, *, #10662, .F. ) ;
#8796 = CIRCLE ( 'NONE', #1668, 27.00000000002699707 ) ;
#8797 = EDGE_CURVE ( 'NONE', #4256, #4485, #8951, .T. ) ;
#8798 = CARTESIAN_POINT ( 'NONE',  ( 2.500000000000000000, 2.357898499370433054, -1.951563910473907981E-15 ) ) ;
#8799 = EDGE_LOOP ( 'NONE', ( #5398, #10782, #10657, #9224 ) ) ;
#8800 = DIRECTION ( 'NONE',  ( 1.000000000000000000, -0.000000000000000000, -0.000000000000000000 ) ) ;
#8801 = DIRECTION ( 'NONE',  ( 0.000000000000000000, 0.000000000000000000, 1.000000000000000000 ) ) ;
#8802 = DIRECTION ( 'NONE',  ( 0.000000000000000000, 0.000000000000000000, 1.000000000000000000 ) ) ;
#8803 = DIRECTION ( 'NONE',  ( 0.000000000000000000, 0.000000000000000000, 1.000000000000000000 ) ) ;
#8804 = VECTOR ( 'NONE', #12252, 1000.000000000000000 ) ;
#8805 = ORIENTED_EDGE ( 'NONE', *, *, #3017, .T. ) ;
#8806 = ORIENTED_EDGE ( 'NONE', *, *, #10379, .T. ) ;
#8807 = EDGE_LOOP ( 'NONE', ( #761, #11088, #960, #4224 ) ) ;
#8808 = DIRECTION ( 'NONE',  ( 0.000000000000000000, -0.5000000000000069944, 0.8660254037844344888 ) ) ;
#8809 = EDGE_LOOP ( 'NONE', ( #4979, #6975, #9099, #3105 ) ) ;
#8810 = CARTESIAN_POINT ( 'NONE',  ( 2.499999999999999556, -4.576198416197066798, -26.60936692326695407 ) ) ;
#8811 =( GEOMETRIC_REPRESENTATION_CONTEXT ( 3 ) GLOBAL_UNCERTAINTY_ASSIGNED_CONTEXT ( ( #8660 ) ) GLOBAL_UNIT_ASSIGNED_CONTEXT ( ( #8708, #6766, #2947 ) ) REPRESENTATION_CONTEXT ( 'NONE', 'WORKASPACE' ) );
#8812 = AXIS2_PLACEMENT_3D ( 'NONE', #3831, #2013, #6767 ) ;
#8813 = CIRCLE ( 'NONE', #9214, 4.000000000000003553 ) ;
#8814 = CARTESIAN_POINT ( 'NONE',  ( 2.500000000000000000, 0.000000000000000000, 2.041999999999999815 ) ) ;
#8815 = APPLICATION_CONTEXT ( 'automotive_design' ) ;
#8816 = EDGE_LOOP ( 'NONE', ( #2925, #7731, #3147, #6565 ) ) ;
#8818 = CARTESIAN_POINT ( 'NONE',  ( -20.63749999999999574, 0.000000000000000000, -6.750000000000000000 ) ) ;
#8817 = AXIS2_PLACEMENT_3D ( 'NONE', #9486, #719, #4532 ) ;
#8819 = DIRECTION ( 'NONE',  ( 1.000000000000000000, 0.000000000000000000, 0.000000000000000000 ) ) ;
#8820 = AXIS2_PLACEMENT_3D ( 'NONE', #4678, #9364, #11346 ) ;
#8821 = ORIENTED_EDGE ( 'NONE', *, *, #6519, .T. ) ;
#8822 = CARTESIAN_POINT ( 'NONE',  ( 70.79898987322334847, -3.499999999999998668, -45.49999999999998579 ) ) ;
#8823 = AXIS2_PLACEMENT_3D ( 'NONE', #8684, #107, #7742 ) ;
#8824 = CARTESIAN_POINT ( 'NONE',  ( 4.999999999999999112, 13.85025647830082818, -17.79862902732250163 ) ) ;
#8825 = CIRCLE ( 'NONE', #11000, 7.200000000007204193 ) ;
#8826 = CARTESIAN_POINT ( 'NONE',  ( 33.00000000000000000, 0.000000000000000000, 0.000000000000000000 ) ) ;
#8827 = EDGE_CURVE ( 'NONE', #11534, #8402, #8899, .T. ) ;
#8828 = ORIENTED_EDGE ( 'NONE', *, *, #1496, .T. ) ;
#8829 = DIRECTION ( 'NONE',  ( 0.000000000000000000, -0.8660254037844390407, -0.4999999999999994449 ) ) ;
#8830 = EDGE_CURVE ( 'NONE', #8354, #2097, #7416, .T. ) ;
#8831 = STYLED_ITEM ( 'NONE', ( #8945 ), #11675 ) ;
#8832 = CIRCLE ( 'NONE', #7437, 4.250000000000000000 ) ;
#8833 = CIRCLE ( 'NONE', #11013, 4.000000000000003553 ) ;
#8834 = CIRCLE ( 'NONE', #4824, 40.00000000000000711 ) ;
#8835 = AXIS2_PLACEMENT_3D ( 'NONE', #8101, #7026, #11826 ) ;
#8836 =( NAMED_UNIT ( * ) PLANE_ANGLE_UNIT ( ) SI_UNIT ( $, .RADIAN. ) );
#8837 = DIRECTION ( 'NONE',  ( -1.000000000000000000, -0.000000000000000000, 0.000000000000000000 ) ) ;
#8838 = DIRECTION ( 'NONE',  ( 0.000000000000000000, 0.000000000000000000, 1.000000000000000000 ) ) ;
#8839 = LINE ( 'NONE', #4947, #6447 ) ;
#8840 = EDGE_LOOP ( 'NONE', ( #2970, #6995, #151, #3052 ) ) ;
#8841 = FACE_OUTER_BOUND ( 'NONE', #3020, .T. ) ;
#8842 = DIRECTION ( 'NONE',  ( -1.000000000000000000, -0.000000000000000000, 0.000000000000000000 ) ) ;
#8843 =( GEOMETRIC_REPRESENTATION_CONTEXT ( 3 ) GLOBAL_UNCERTAINTY_ASSIGNED_CONTEXT ( ( #1017 ) ) GLOBAL_UNIT_ASSIGNED_CONTEXT ( ( #6880, #1233, #5054 ) ) REPRESENTATION_CONTEXT ( 'NONE', 'WORKASPACE' ) );
#8844 = VECTOR ( 'NONE', #4574, 1000.000000000000000 ) ;
#8845 = VERTEX_POINT ( 'NONE', #7838 ) ;
#8846 = CARTESIAN_POINT ( 'NONE',  ( -36.00000000000000000, 34.64101615137756340, -19.99999999999998934 ) ) ;
#8847 = CIRCLE ( 'NONE', #4437, 21.00000000002100009 ) ;
#8848 = EDGE_CURVE ( 'NONE', #1870, #10292, #6950, .T. ) ;
#8849 = CIRCLE ( 'NONE', #841, 7.200000000007202416 ) ;
#8850 = ORIENTED_EDGE ( 'NONE', *, *, #174, .F. ) ;
#8851 = DIRECTION ( 'NONE',  ( 0.000000000000000000, 0.000000000000000000, 1.000000000000000000 ) ) ;
#8852 = EDGE_CURVE ( 'NONE', #1528, #6266, #5209, .T. ) ;
#8853 = EDGE_CURVE ( 'NONE', #4341, #11321, #4004, .T. ) ;
#8854 = EDGE_CURVE ( 'NONE', #825, #11527, #2190, .T. ) ;
#8855 = AXIS2_PLACEMENT_3D ( 'NONE', #9929, #9985, #1348 ) ;
#8856 = AXIS2_PLACEMENT_3D ( 'NONE', #1261, #2367, #1313 ) ;
#8857 = CIRCLE ( 'NONE', #10643, 0.7500000000000000000 ) ;
#8858 = FILL_AREA_STYLE_COLOUR ( '', #3609 ) ;
#8859 = CARTESIAN_POINT ( 'NONE',  ( 0.000000000000000000, 0.000000000000000000, 0.000000000000000000 ) ) ;
#8860 = AXIS2_PLACEMENT_3D ( 'NONE', #11437, #9642, #7509 ) ;
#8861 = CARTESIAN_POINT ( 'NONE',  ( 2.500000000000000000, -1.178949249685218303, -2.041999999999998039 ) ) ;
#8862 = DIRECTION ( 'NONE',  ( 0.000000000000000000, 0.000000000000000000, 1.000000000000000000 ) ) ;
#8863 = EDGE_LOOP ( 'NONE', ( #918, #12111, #5939, #9736 ) ) ;
#8864 = DIRECTION ( 'NONE',  ( 1.000000000000000000, 0.000000000000000000, 0.000000000000000000 ) ) ;
#8865 = ORIENTED_EDGE ( 'NONE', *, *, #9751, .T. ) ;
#8866 = FACE_OUTER_BOUND ( 'NONE', #5861, .T. ) ;
#8867 = CONTEXT_DEPENDENT_SHAPE_REPRESENTATION ( #5136, #7039 ) ;
#8868 = ADVANCED_BREP_SHAPE_REPRESENTATION ( '', ( #8661, #6056 ), #3048 ) ;
#8869 = ORIENTED_EDGE ( 'NONE', *, *, #9979, .F. ) ;
#8870 = ADVANCED_FACE ( 'NONE', ( #8670 ), #8727, .T. ) ;
#8871 = AXIS2_PLACEMENT_3D ( 'NONE', #11005, #2371, #6324 ) ;
#8872 = PRODUCT_DEFINITION ( 'UNKNOWN', '', #6443, #11644 ) ;
#8873 = EDGE_LOOP ( 'NONE', ( #7598, #3204, #10, #9746 ) ) ;
#8874 = ORIENTED_EDGE ( 'NONE', *, *, #6476, .T. ) ;
#8875 = CARTESIAN_POINT ( 'NONE',  ( 0.000000000000000000, 2.357898499370433054, -1.951563910473907981E-15 ) ) ;
#8876 = FACE_OUTER_BOUND ( 'NONE', #8621, .T. ) ;
#8877 = DIRECTION ( 'NONE',  ( 0.000000000000000000, 0.000000000000000000, 1.000000000000000000 ) ) ;
#8878 = CARTESIAN_POINT ( 'NONE',  ( 4.999999999999997335, 4.769696007084728073, 1.500000000000000000 ) ) ;
#8879 = ORIENTED_EDGE ( 'NONE', *, *, #343, .T. ) ;
#8880 = VECTOR ( 'NONE', #2745, 1000.000000000000000 ) ;
#8881 = VERTEX_POINT ( 'NONE', #6012 ) ;
#8882 = EDGE_CURVE ( 'NONE', #6667, #2734, #7210, .T. ) ;
#8884 = ADVANCED_FACE ( 'NONE', ( #6077 ), #1368, .T. ) ;
#8883 = ORIENTED_EDGE ( 'NONE', *, *, #5496, .F. ) ;
#8885 = DIRECTION ( 'NONE',  ( 0.000000000000000000, 0.000000000000000000, 1.000000000000000000 ) ) ;
#8886 = CARTESIAN_POINT ( 'NONE',  ( 1.500000000000001332, 0.000000000000000000, -7.399999999999999467 ) ) ;
#8887 = CIRCLE ( 'NONE', #6079, 5.000000000000000000 ) ;
#8888 = CARTESIAN_POINT ( 'NONE',  ( 4.999999999999999112, 22.37914155802285876, -2.791921004064323864 ) ) ;
#8889 = ORIENTED_EDGE ( 'NONE', *, *, #1294, .T. ) ;
#8890 = DIRECTION ( 'NONE',  ( 1.000000000000000000, 0.000000000000000000, 0.000000000000000000 ) ) ;
#8891 = CARTESIAN_POINT ( 'NONE',  ( 4.999999999999999112, -14.40062958310459251, -8.872489362018340486 ) ) ;
#8892 = ORIENTED_EDGE ( 'NONE', *, *, #1420, .T. ) ;
#8893 = CIRCLE ( 'NONE', #3492, 20.24900000002024925 ) ;
#8894 = DIRECTION ( 'NONE',  ( 1.000000000000000000, 0.000000000000000000, 0.000000000000000000 ) ) ;
#8895 = DIRECTION ( 'NONE',  ( 0.000000000000000000, 0.000000000000000000, 1.000000000000000000 ) ) ;
#8896 = EDGE_LOOP ( 'NONE', ( #11766, #2693, #2321, #6535, #5879 ) ) ;
#8897 = DIRECTION ( 'NONE',  ( 0.000000000000000000, 0.000000000000000000, 1.000000000000000000 ) ) ;
#8898 = CIRCLE ( 'NONE', #3906, 5.000000000000000000 ) ;
#8899 = LINE ( 'NONE', #4005, #608 ) ;
#8900 = DIRECTION ( 'NONE',  ( -1.000000000000000000, -0.000000000000000000, 0.000000000000000000 ) ) ;
#8901 = DIRECTION ( 'NONE',  ( 1.000000000000000000, 0.000000000000000000, 0.000000000000000000 ) ) ;
#8902 = CARTESIAN_POINT ( 'NONE',  ( 4.999999999999999112, -14.88411597386723351, -8.035066368449358620 ) ) ;
#8903 = VERTEX_POINT ( 'NONE', #8085 ) ;
#8904 = ADVANCED_FACE ( 'NONE', ( #11869 ), #2365, .F. ) ;
#8905 = DIRECTION ( 'NONE',  ( -1.000000000000000000, -0.000000000000000000, 0.000000000000000000 ) ) ;
#8906 = DIRECTION ( 'NONE',  ( -1.000000000000000000, 0.000000000000000000, 0.000000000000000000 ) ) ;
#8907 = SHAPE_REPRESENTATION ( 'main body', ( #6056 ), #6251 ) ;
#8908 = ORIENTED_EDGE ( 'NONE', *, *, #10428, .F. ) ;
#8909 = CARTESIAN_POINT ( 'NONE',  ( 0.000000000000000000, -0.5999999999999996447, -2.622672778259560467 ) ) ;
#8910 = VERTEX_POINT ( 'NONE', #3681 ) ;
#8911 = DIRECTION ( 'NONE',  ( 0.000000000000000000, -0.7071067811865537900, 0.7071067811865414665 ) ) ;
#8912 = DIRECTION ( 'NONE',  ( 0.000000000000000000, 0.000000000000000000, 1.000000000000000000 ) ) ;
#8913 = EDGE_CURVE ( 'NONE', #7918, #2661, #6612, .T. ) ;
#8914 = DIRECTION ( 'NONE',  ( 0.000000000000000000, 0.000000000000000000, 1.000000000000000000 ) ) ;
#8915 = DIRECTION ( 'NONE',  ( -1.000000000000000000, 0.000000000000000000, 0.000000000000000000 ) ) ;
#8916 = ORIENTED_EDGE ( 'NONE', *, *, #3179, .T. ) ;
#8917 = EDGE_CURVE ( 'NONE', #972, #9795, #10301, .T. ) ;
#8918 = ADVANCED_FACE ( 'NONE', ( #1930 ), #8137, .T. ) ;
#8919 = ORIENTED_EDGE ( 'NONE', *, *, #7333, .F. ) ;
#8920 = CARTESIAN_POINT ( 'NONE',  ( 0.000000000000000000, 11.41582255376072830, 8.527191590521114861 ) ) ;
#8921 = ITEM_DEFINED_TRANSFORMATION ( 'NONE', 'NONE', #6053,  #6056 ) ;
#8922 = ORIENTED_EDGE ( 'NONE', *, *, #3699, .F. ) ;
#8923 = DIRECTION ( 'NONE',  ( 0.000000000000000000, -1.000000000000000000, 0.000000000000000000 ) ) ;
#8924 = CARTESIAN_POINT ( 'NONE',  ( 4.999999999999999112, -17.79862902732255137, -13.85025647830076245 ) ) ;
#8925 = CYLINDRICAL_SURFACE ( 'NONE', #4008, 7.200000000007202416 ) ;
#8926 = FACE_OUTER_BOUND ( 'NONE', #1513, .T. ) ;
#8927 = CARTESIAN_POINT ( 'NONE',  ( 0.000000000000000000, -21.74405275335762155, 5.984728032764886407 ) ) ;
#8928 = VERTEX_POINT ( 'NONE', #7498 ) ;
#8929 = EDGE_CURVE ( 'NONE', #8510, #2345, #9137, .T. ) ;
#8930 = DIRECTION ( 'NONE',  ( 0.000000000000000000, 0.000000000000000000, -1.000000000000000000 ) ) ;
#8931 = EDGE_CURVE ( 'NONE', #9683, #1657, #1795, .T. ) ;
#8932 = ORIENTED_EDGE ( 'NONE', *, *, #6661, .F. ) ;
#8933 = ORIENTED_EDGE ( 'NONE', *, *, #4270, .T. ) ;
#8934 = CARTESIAN_POINT ( 'NONE',  ( -20.00000000000000000, 0.000000000000000000, 0.000000000000000000 ) ) ;
#8935 = PRODUCT_DEFINITION_SHAPE ( 'NONE', 'NONE',  #12353 ) ;
#8936 = CARTESIAN_POINT ( 'NONE',  ( 4.999999999999999112, 2.791921004064568113, -22.37914155802282323 ) ) ;
#8937 = CARTESIAN_POINT ( 'NONE',  ( 42.00000000000000000, -0.8169585525225422362, -40.74199414808185793 ) ) ;
#8938 = EDGE_CURVE ( 'NONE', #394, #10134, #10804, .T. ) ;
#8939 = EDGE_CURVE ( 'NONE', #9414, #7555, #920, .T. ) ;
#8940 = ORIENTED_EDGE ( 'NONE', *, *, #6661, .T. ) ;
#8941 = LINE ( 'NONE', #8818, #9564 ) ;
#8942 = CARTESIAN_POINT ( 'NONE',  ( 2.499999999999999556, -14.41081992069326034, 22.83261415639497471 ) ) ;
#8943 = ORIENTED_EDGE ( 'NONE', *, *, #2101, .T. ) ;
#8944 = FACE_OUTER_BOUND ( 'NONE', #12175, .T. ) ;
#8945 = PRESENTATION_STYLE_ASSIGNMENT (( #182 ) ) ;
#8946 = DIRECTION ( 'NONE',  ( 1.000000000000000000, 0.000000000000000000, 0.000000000000000000 ) ) ;
#8947 = CARTESIAN_POINT ( 'NONE',  ( 36.00000000000000711, 0.000000000000000000, 40.00000000000000711 ) ) ;
#8948 = ORIENTED_EDGE ( 'NONE', *, *, #5115, .T. ) ;
#8949 = DIRECTION ( 'NONE',  ( 1.000000000000000000, -0.000000000000000000, -0.000000000000000000 ) ) ;
#8950 = DIRECTION ( 'NONE',  ( 0.000000000000000000, 0.000000000000000000, 1.000000000000000000 ) ) ;
#8951 = LINE ( 'NONE', #5950, #10795 ) ;
#8952 = LINE ( 'NONE', #7839, #9606 ) ;
#8953 = CARTESIAN_POINT ( 'NONE',  ( 36.00000000000000711, 0.000000000000000000, 0.000000000000000000 ) ) ;
#8954 = CARTESIAN_POINT ( 'NONE',  ( 0.000000000000000000, 4.916402349214870071, -20.41639017900854469 ) ) ;
#8955 = ORIENTED_EDGE ( 'NONE', *, *, #595, .T. ) ;
#8956 = ORIENTED_EDGE ( 'NONE', *, *, #7910, .T. ) ;
#8957 = CARTESIAN_POINT ( 'NONE',  ( 36.00000000000000711, 1.456773409934505593E-31, -41.99999999999998579 ) ) ;
#8958 = CARTESIAN_POINT ( 'NONE',  ( 37.00000000000000711, -3.277848209564065307, -45.50652407877909411 ) ) ;
#8959 = ORIENTED_EDGE ( 'NONE', *, *, #3540, .F. ) ;
#8960 = FACE_OUTER_BOUND ( 'NONE', #2629, .T. ) ;
#8961 = ORIENTED_EDGE ( 'NONE', *, *, #4110, .F. ) ;
#8962 = DIRECTION ( 'NONE',  ( 1.000000000000000000, -0.000000000000000000, -0.000000000000000000 ) ) ;
#8963 = VECTOR ( 'NONE', #7130, 1000.000000000000000 ) ;
#8964 = CIRCLE ( 'NONE', #1556, 4.799999999999999822 ) ;
#8965 = CARTESIAN_POINT ( 'NONE',  ( 4.999999999999999112, -22.37914155802283034, -2.791921004064479739 ) ) ;
#8966 = CARTESIAN_POINT ( 'NONE',  ( -15.00000000000000000, 40.00000000000000711, 0.000000000000000000 ) ) ;
#8967 = FACE_OUTER_BOUND ( 'NONE', #7309, .T. ) ;
#8968 = CARTESIAN_POINT ( 'NONE',  ( -1.500000000000000888, 0.000000000000000000, -5.100000000000000533 ) ) ;
#8969 = AXIS2_PLACEMENT_3D ( 'NONE', #9695, #5058, #2237 ) ;
#8970 = AXIS2_PLACEMENT_3D ( 'NONE', #4441, #1505, #8269 ) ;
#8971 = ORIENTED_EDGE ( 'NONE', *, *, #189, .T. ) ;
#8972 = DIRECTION ( 'NONE',  ( -0.000000000000000000, -0.000000000000000000, 1.000000000000000000 ) ) ;
#8973 = ORIENTED_EDGE ( 'NONE', *, *, #790, .F. ) ;
#8974 = CARTESIAN_POINT ( 'NONE',  ( 5.200000000000002842, 3.306546357697854226E-16, 2.700000000000000622 ) ) ;
#8975 = ORIENTED_EDGE ( 'NONE', *, *, #10662, .T. ) ;
#8976 = EDGE_CURVE ( 'NONE', #7774, #4444, #4822, .T. ) ;
#8977 = TOROIDAL_SURFACE ( 'NONE', #5974, 2.690429798716874377, 1.199999999999999956 ) ;
#8978 = VECTOR ( 'NONE', #10120, 999.9999999999998863 ) ;
#8979 = EDGE_CURVE ( 'NONE', #3971, #825, #4627, .T. ) ;
#8980 = FACE_OUTER_BOUND ( 'NONE', #9156, .T. ) ;
#8981 = AXIS2_PLACEMENT_3D ( 'NONE', #7593, #1966, #9591 ) ;
#8982 = CARTESIAN_POINT ( 'NONE',  ( 15.00000000000000355, 44.00000000000001421, -2.149999999999999023 ) ) ;
#8983 = DIRECTION ( 'NONE',  ( 0.000000000000000000, 0.5068368027542899945, -0.8620420264545162192 ) ) ;
#8984 = CARTESIAN_POINT ( 'NONE',  ( 0.000000000000000000, 0.000000000000000000, 0.000000000000000000 ) ) ;
#8985 = DIRECTION ( 'NONE',  ( -1.000000000000000000, -0.000000000000000000, 0.000000000000000000 ) ) ;
#8986 = EDGE_LOOP ( 'NONE', ( #11961, #4655, #12174, #2442 ) ) ;
#8987 = DIRECTION ( 'NONE',  ( 1.000000000000000000, -0.000000000000000000, 0.000000000000000000 ) ) ;
#8988 = ORIENTED_EDGE ( 'NONE', *, *, #4498, .T. ) ;
#8989 = AXIS2_PLACEMENT_3D ( 'NONE', #12306, #2818, #5896 ) ;
#8990 = DIRECTION ( 'NONE',  ( 0.000000000000000000, 0.000000000000000000, 1.000000000000000000 ) ) ;
#8991 = VERTEX_POINT ( 'NONE', #12287 ) ;
#8992 = AXIS2_PLACEMENT_3D ( 'NONE', #1907, #12319, #11392 ) ;
#8993 = DIRECTION ( 'NONE',  ( 1.000000000000000000, -0.000000000000000000, 0.000000000000000000 ) ) ;
#8994 = EDGE_CURVE ( 'NONE', #3875, #5016, #1733, .T. ) ;
#8995 = CARTESIAN_POINT ( 'NONE',  ( 10.00000000000000711, 44.00000000000001421, -12.50000000000000000 ) ) ;
#8996 = ADVANCED_FACE ( 'NONE', ( #3736 ), #5427, .T. ) ;
#8997 = ADVANCED_FACE ( 'NONE', ( #2438 ), #12344, .F. ) ;
#8998 = EDGE_CURVE ( 'NONE', #10979, #7124, #4364, .T. ) ;
#8999 = VECTOR ( 'NONE', #2469, 1000.000000000000000 ) ;
#9000 = CARTESIAN_POINT ( 'NONE',  ( -1.500000000000001332, 0.000000000000000000, -7.399999999999999467 ) ) ;
#9001 = AXIS2_PLACEMENT_3D ( 'NONE', #8446, #11487, #3932 ) ;
#9002 = ORIENTED_EDGE ( 'NONE', *, *, #192, .T. ) ;
#9003 = CARTESIAN_POINT ( 'NONE',  ( 51.00000000000000000, 46.00000000000001421, -41.99999999999999289 ) ) ;
#9004 = ORIENTED_EDGE ( 'NONE', *, *, #1554, .T. ) ;
#9005 = SURFACE_STYLE_FILL_AREA ( #250 ) ;
#9006 = CARTESIAN_POINT ( 'NONE',  ( 20.00000000000000000, 0.000000000000000000, 0.000000000000000000 ) ) ;
#9007 =( GEOMETRIC_REPRESENTATION_CONTEXT ( 3 ) GLOBAL_UNCERTAINTY_ASSIGNED_CONTEXT ( ( #4393 ) ) GLOBAL_UNIT_ASSIGNED_CONTEXT ( ( #513, #11700, #4267 ) ) REPRESENTATION_CONTEXT ( 'NONE', 'WORKASPACE' ) );
#9008 = CYLINDRICAL_SURFACE ( 'NONE', #7907, 27.00000000002699707 ) ;
#9009 = EDGE_CURVE ( 'NONE', #4033, #1905, #858, .T. ) ;
#9010 = AXIS2_PLACEMENT_3D ( 'NONE', #8138, #7327, #6374 ) ;
#9011 = ORIENTED_EDGE ( 'NONE', *, *, #979, .F. ) ;
#9012 = DIRECTION ( 'NONE',  ( 0.000000000000000000, 0.000000000000000000, -1.000000000000000000 ) ) ;
#9013 = TOROIDAL_SURFACE ( 'NONE', #11587, 6.250000000000000000, 0.7500000000000000000 ) ;
#9014 = MECHANICAL_DESIGN_GEOMETRIC_PRESENTATION_REPRESENTATION (  '', ( #2607 ), #8811 ) ;
#9015 = AXIS2_PLACEMENT_3D ( 'NONE', #4520, #894, #8526 ) ;
#9016 = DIRECTION ( 'NONE',  ( 1.000000000000000000, 0.000000000000000000, 0.000000000000000000 ) ) ;
#9017 = DIRECTION ( 'NONE',  ( 1.000000000000000000, 0.000000000000000000, 0.000000000000000000 ) ) ;
#9018 = AXIS2_PLACEMENT_3D ( 'NONE', #5873, #162, #4340 ) ;
#9019 = AXIS2_PLACEMENT_3D ( 'NONE', #12028, #10221, #7480 ) ;
#9020 = AXIS2_PLACEMENT_3D ( 'NONE', #779, #11228, #205 ) ;
#9021 = DIRECTION ( 'NONE',  ( 0.000000000000000000, 0.000000000000000000, -1.000000000000000000 ) ) ;
#9022 = LINE ( 'NONE', #8769, #439 ) ;
#9023 = EDGE_LOOP ( 'NONE', ( #9075, #1301 ) ) ;
#9024 = ORIENTED_EDGE ( 'NONE', *, *, #6937, .T. ) ;
#9025 = CARTESIAN_POINT ( 'NONE',  ( 0.000000000000000000, 0.000000000000000000, 0.000000000000000000 ) ) ;
#9026 = CARTESIAN_POINT ( 'NONE',  ( 36.00000000000000711, -12.50000000000000000, -37.99671038392666134 ) ) ;
#9027 = ORIENTED_EDGE ( 'NONE', *, *, #10658, .F. ) ;
#9028 = CARTESIAN_POINT ( 'NONE',  ( 51.00000000000000000, 0.000000000000000000, -41.99999999999999289 ) ) ;
#9029 = PRODUCT_DEFINITION_CONTEXT ( 'detailed design', #493, 'design' ) ;
#9030 = ADVANCED_FACE ( 'NONE', ( #5547 ), #9497, .F. ) ;
#9031 = VERTEX_POINT ( 'NONE', #9686 ) ;
#9032 = DIRECTION ( 'NONE',  ( -1.000000000000000000, 0.000000000000000000, 0.000000000000000000 ) ) ;
#9033 = EDGE_CURVE ( 'NONE', #10418, #4328, #10996, .T. ) ;
#9034 = MECHANICAL_DESIGN_GEOMETRIC_PRESENTATION_REPRESENTATION (  '', ( #4028 ), #5621 ) ;
#9035 = CIRCLE ( 'NONE', #6835, 5.525000000000000355 ) ;
#9036 = CIRCLE ( 'NONE', #9441, 7.200000000007203305 ) ;
#9037 = VECTOR ( 'NONE', #8034, 1000.000000000000000 ) ;
#9038 = FACE_OUTER_BOUND ( 'NONE', #1150, .T. ) ;
#9039 = DIRECTION ( 'NONE',  ( 1.000000000000000000, -0.000000000000000000, 0.000000000000000000 ) ) ;
#9040 =( GEOMETRIC_REPRESENTATION_CONTEXT ( 3 ) GLOBAL_UNCERTAINTY_ASSIGNED_CONTEXT ( ( #9663 ) ) GLOBAL_UNIT_ASSIGNED_CONTEXT ( ( #10122, #5366, #543 ) ) REPRESENTATION_CONTEXT ( 'NONE', 'WORKASPACE' ) );
#9041 = CARTESIAN_POINT ( 'NONE',  ( 4.999999999999999112, -11.14352537685160982, -19.60720892790264713 ) ) ;
#9042 = CARTESIAN_POINT ( 'NONE',  ( 36.00000000000000711, -3.403685371105885427, -38.61548734756097190 ) ) ;
#9043 = CIRCLE ( 'NONE', #435, 14.24900000001425227 ) ;
#9044 = CIRCLE ( 'NONE', #6044, 7.500000000000000000 ) ;
#9045 = PRODUCT_DEFINITION_SHAPE ( 'NONE', 'NONE',  #12369 ) ;
#9046 = ORIENTED_EDGE ( 'NONE', *, *, #10893, .T. ) ;
#9047 = VECTOR ( 'NONE', #7901, 1000.000000000000000 ) ;
#9048 = DIRECTION ( 'NONE',  ( -1.000000000000000000, -0.000000000000000000, -0.000000000000000000 ) ) ;
#9049 = ORIENTED_EDGE ( 'NONE', *, *, #7592, .T. ) ;
#9050 = SURFACE_STYLE_USAGE ( .BOTH. , #9915 ) ;
#9051 = ORIENTED_EDGE ( 'NONE', *, *, #7095, .T. ) ;
#9052 = CARTESIAN_POINT ( 'NONE',  ( 33.00000000000000000, 0.000000000000000000, -49.49999999999999289 ) ) ;
#9053 = CIRCLE ( 'NONE', #10425, 20.24900000002024569 ) ;
#9054 = AXIS2_PLACEMENT_3D ( 'NONE', #2441, #8379, #6195 ) ;
#9055 = CARTESIAN_POINT ( 'NONE',  ( 1.600000000000000089, 0.000000000000000000, 0.000000000000000000 ) ) ;
#9056 = DIRECTION ( 'NONE',  ( 0.000000000000000000, -0.8660254037844328234, -0.5000000000000099920 ) ) ;
#9057 = DIRECTION ( 'NONE',  ( 0.000000000000000000, 0.4999999999999993339, -0.8660254037844390407 ) ) ;
#9058 = PLANE ( 'NONE',  #5220 ) ;
#9059 = DIRECTION ( 'NONE',  ( -1.000000000000000000, 0.000000000000000000, 0.000000000000000000 ) ) ;
#9060 = EDGE_CURVE ( 'NONE', #3460, #11522, #976, .T. ) ;
#9061 = ORIENTED_EDGE ( 'NONE', *, *, #1536, .F. ) ;
#9062 = CARTESIAN_POINT ( 'NONE',  ( 37.00000000000000711, -3.403685371105885427, -38.61548734756097190 ) ) ;
#9063 = AXIS2_PLACEMENT_3D ( 'NONE', #3949, #7768, #11558 ) ;
#9064 = VERTEX_POINT ( 'NONE', #6873 ) ;
#9065 = EDGE_CURVE ( 'NONE', #8440, #353, #6030, .T. ) ;
#9066 = DIRECTION ( 'NONE',  ( 0.000000000000000000, 0.000000000000000000, 1.000000000000000000 ) ) ;
#9067 = VECTOR ( 'NONE', #8753, 1000.000000000000000 ) ;
#9068 = VERTEX_POINT ( 'NONE', #11530 ) ;
#9069 = DIRECTION ( 'NONE',  ( 1.000000000000000000, 0.000000000000000000, 0.000000000000000000 ) ) ;
#9070 = DIRECTION ( 'NONE',  ( 1.000000000000000000, 0.000000000000000000, 0.000000000000000000 ) ) ;
#9071 = ORIENTED_EDGE ( 'NONE', *, *, #914, .T. ) ;
#9072 = DIRECTION ( 'NONE',  ( 0.000000000000000000, 0.000000000000000000, 1.000000000000000000 ) ) ;
#9073=STYLED_ITEM('',(#12398),#4380);
#9074 = EDGE_CURVE ( 'NONE', #11627, #451, #8624, .T. ) ;
#9075 = ORIENTED_EDGE ( 'NONE', *, *, #7230, .T. ) ;
#9076 = LINE ( 'NONE', #4242, #1365 ) ;
#9077 = EDGE_LOOP ( 'NONE', ( #9925, #4552 ) ) ;
#9078 = ADVANCED_FACE ( 'NONE', ( #3169 ), #9740, .F. ) ;
#9079 = EDGE_CURVE ( 'NONE', #8025, #3605, #10677, .T. ) ;
#9080 = DIRECTION ( 'NONE',  ( -1.000000000000000000, -0.000000000000000000, -0.000000000000000000 ) ) ;
#9081 = AXIS2_PLACEMENT_3D ( 'NONE', #6403, #6473, #10271 ) ;
#9082 = EDGE_LOOP ( 'NONE', ( #7371, #10066 ) ) ;
#9083 = DIRECTION ( 'NONE',  ( -1.000000000000000000, 0.000000000000000000, -0.000000000000000000 ) ) ;
#9084 = DIRECTION ( 'NONE',  ( 0.000000000000000000, -0.3826834323650971648, 0.9238795325112837409 ) ) ;
#9085 = DIRECTION ( 'NONE',  ( -1.000000000000000000, -0.000000000000000000, -0.000000000000000000 ) ) ;
#9086 = DIRECTION ( 'NONE',  ( -1.000000000000000000, -0.000000000000000000, 0.000000000000000000 ) ) ;
#9087 = AXIS2_PLACEMENT_3D ( 'NONE', #270, #4083, #6139 ) ;
#9088 = CARTESIAN_POINT ( 'NONE',  ( 4.999999999999999112, -14.14998813191270877, 1.676853263447836584 ) ) ;
#9089 = CARTESIAN_POINT ( 'NONE',  ( -15.00000000000000000, 40.00000000000000711, 0.000000000000000000 ) ) ;
#9090 = ORIENTED_EDGE ( 'NONE', *, *, #10953, .T. ) ;
#9091 = ORIENTED_EDGE ( 'NONE', *, *, #6452, .F. ) ;
#9092 = CARTESIAN_POINT ( 'NONE',  ( 42.00000000000000000, 4.814824860968089633E-32, 0.000000000000000000 ) ) ;
#9093 = CARTESIAN_POINT ( 'NONE',  ( 2.595115354961440524, -7.673029147243177306, -1.000000000000000000 ) ) ;
#9094 = VERTEX_POINT ( 'NONE', #7802 ) ;
#9095 = FACE_OUTER_BOUND ( 'NONE', #5875, .T. ) ;
#9096 = ORIENTED_EDGE ( 'NONE', *, *, #6557, .T. ) ;
#9097 = FACE_OUTER_BOUND ( 'NONE', #5196, .T. ) ;
#9098 = CIRCLE ( 'NONE', #1298, 6.500000000000000888 ) ;
#9099 = ORIENTED_EDGE ( 'NONE', *, *, #6529, .F. ) ;
#9100 = SURFACE_STYLE_USAGE ( .BOTH. , #6963 ) ;
#9101 = CARTESIAN_POINT ( 'NONE',  ( 51.00000000000000000, 3.500000000000001332, -45.49999999999998579 ) ) ;
#9102 = EDGE_CURVE ( 'NONE', #7542, #10266, #11475, .T. ) ;
#9103 = EDGE_CURVE ( 'NONE', #10134, #3361, #229, .T. ) ;
#9104 = DIRECTION ( 'NONE',  ( 1.000000000000000000, 0.000000000000000000, 0.000000000000000000 ) ) ;
#9105 = CYLINDRICAL_SURFACE ( 'NONE', #11619, 9.600000000009600853 ) ;
#9106 = ORIENTED_EDGE ( 'NONE', *, *, #6390, .T. ) ;
#9107 = DIRECTION ( 'NONE',  ( 0.000000000000000000, 0.000000000000000000, 1.000000000000000000 ) ) ;
#9108 = AXIS2_PLACEMENT_3D ( 'NONE', #865, #56, #927 ) ;
#9109 = CARTESIAN_POINT ( 'NONE',  ( 4.999999999999999112, -15.57980286237488343, 22.05152472667124286 ) ) ;
#9110 = ORIENTED_EDGE ( 'NONE', *, *, #1879, .T. ) ;
#9111 = CARTESIAN_POINT ( 'NONE',  ( 43.00000000000000000, 3.903127820947864496E-18, 0.000000000000000000 ) ) ;
#9112 = VERTEX_POINT ( 'NONE', #4918 ) ;
#9113 = LINE ( 'NONE', #10274, #11556 ) ;
#9114 = DIRECTION ( 'NONE',  ( -1.000000000000000000, -0.000000000000000000, 0.000000000000000000 ) ) ;
#9115 = FACE_OUTER_BOUND ( 'NONE', #9863, .T. ) ;
#9116 = DIRECTION ( 'NONE',  ( -1.000000000000000000, -0.000000000000000000, -0.000000000000000000 ) ) ;
#9117 = CARTESIAN_POINT ( 'NONE',  ( 4.999999999999997335, 6.799999999999999822, -1.500000000000000000 ) ) ;
#9118 = ORIENTED_EDGE ( 'NONE', *, *, #9009, .F. ) ;
#9119 = FACE_OUTER_BOUND ( 'NONE', #7544, .T. ) ;
#9120 = ORIENTED_EDGE ( 'NONE', *, *, #11426, .T. ) ;
#9121 = DIRECTION ( 'NONE',  ( -0.9999999999999998890, 0.000000000000000000, 0.000000000000000000 ) ) ;
#9122 = ORIENTED_EDGE ( 'NONE', *, *, #7709, .T. ) ;
#9123 = DIRECTION ( 'NONE',  ( 0.000000000000000000, 0.000000000000000000, -1.000000000000000000 ) ) ;
#9124 = CARTESIAN_POINT ( 'NONE',  ( -33.00000000000000000, -9.184850993605149917E-16, 7.500000000000000888 ) ) ;
#9125 = EDGE_LOOP ( 'NONE', ( #4278, #8685, #10542, #7675 ) ) ;
#9126 = LINE ( 'NONE', #5169, #11574 ) ;
#9127 = ORIENTED_EDGE ( 'NONE', *, *, #7458, .T. ) ;
#9128 = CARTESIAN_POINT ( 'NONE',  ( -26.00000000000000355, 0.000000000000000000, 0.000000000000000000 ) ) ;
#9129 = ORIENTED_EDGE ( 'NONE', *, *, #11783, .F. ) ;
#9130 = CYLINDRICAL_SURFACE ( 'NONE', #304, 27.00000000002699707 ) ;
#9131 = ORIENTED_EDGE ( 'NONE', *, *, #11174, .T. ) ;
#9132 = DIRECTION ( 'NONE',  ( -1.000000000000000000, 0.000000000000000000, 0.000000000000000000 ) ) ;
#9133 = EDGE_CURVE ( 'NONE', #2147, #8289, #6979, .T. ) ;
#9134 = PRODUCT ( 'spool', 'spool', '', ( #5035 ) ) ;
#9135 =( NAMED_UNIT ( * ) PLANE_ANGLE_UNIT ( ) SI_UNIT ( $, .RADIAN. ) );
#9136 = EDGE_CURVE ( 'NONE', #558, #1430, #6744, .T. ) ;
#9137 = LINE ( 'NONE', #3446, #2822 ) ;
#9138 = PLANE ( 'NONE',  #9010 ) ;
#9139 = DIRECTION ( 'NONE',  ( -1.000000000000000000, 0.000000000000000000, 0.000000000000000000 ) ) ;
#9140 = DIRECTION ( 'NONE',  ( 0.000000000000000000, 0.000000000000000000, -1.000000000000000000 ) ) ;
#9141 = ORIENTED_EDGE ( 'NONE', *, *, #645, .F. ) ;
#9142 = ORIENTED_EDGE ( 'NONE', *, *, #9595, .T. ) ;
#9143 = DIRECTION ( 'NONE',  ( 0.000000000000000000, 0.7900737791495477946, 0.6130117645692876316 ) ) ;
#9144 = FACE_OUTER_BOUND ( 'NONE', #2460, .T. ) ;
#9145 = ORIENTED_EDGE ( 'NONE', *, *, #4227, .F. ) ;
#9146 = FACE_BOUND ( 'NONE', #2669, .T. ) ;
#9147 = VERTEX_POINT ( 'NONE', #5733 ) ;
#9148 = LINE ( 'NONE', #3385, #4998 ) ;
#9149 = EDGE_CURVE ( 'NONE', #1032, #8188, #5827, .T. ) ;
#9150 = EDGE_CURVE ( 'NONE', #31, #6433, #9551, .T. ) ;
#9151 = EDGE_CURVE ( 'NONE', #9383, #6055, #11398, .T. ) ;
#9152 = FACE_BOUND ( 'NONE', #166, .T. ) ;
#9153 = CARTESIAN_POINT ( 'NONE',  ( 4.999999999999999112, 15.37949036966230132, -13.17168466712912434 ) ) ;
#9154 = LINE ( 'NONE', #10846, #6444 ) ;
#9155 = DIRECTION ( 'NONE',  ( 0.000000000000000000, 0.000000000000000000, 1.000000000000000000 ) ) ;
#9156 = EDGE_LOOP ( 'NONE', ( #5361, #690, #6795, #2369 ) ) ;
#9157 = CARTESIAN_POINT ( 'NONE',  ( -31.74999999999995737, 3.061616997868383634E-16, -2.500000000000000444 ) ) ;
#9158 = CARTESIAN_POINT ( 'NONE',  ( 0.2499999999999966416, -8.096141056083448362, -1.000000000000000000 ) ) ;
#9159 = EDGE_LOOP ( 'NONE', ( #10493, #8278, #5910, #11847 ) ) ;
#9160 =( NAMED_UNIT ( * ) PLANE_ANGLE_UNIT ( ) SI_UNIT ( $, .RADIAN. ) );
#9161 = UNCERTAINTY_MEASURE_WITH_UNIT (LENGTH_MEASURE( 1.000000000000000082E-05 ), #494, 'distance_accuracy_value', 'NONE');
#9162 = ORIENTED_EDGE ( 'NONE', *, *, #4551, .F. ) ;
#9163 = EDGE_CURVE ( 'NONE', #11283, #8451, #6427, .T. ) ;
#9164 = DIRECTION ( 'NONE',  ( 0.000000000000000000, -1.287488025362403787E-15, -1.000000000000000000 ) ) ;
#9165 = VECTOR ( 'NONE', #1877, 1000.000000000000000 ) ;
#9166 = CARTESIAN_POINT ( 'NONE',  ( 1.600000000000000089, 0.000000000000000000, 0.000000000000000000 ) ) ;
#9167 = CARTESIAN_POINT ( 'NONE',  ( -36.00000000000000711, 34.64101615137755630, 20.00000000000001066 ) ) ;
#9168 = AXIS2_PLACEMENT_3D ( 'NONE', #10368, #1810, #5625 ) ;
#9169 = CIRCLE ( 'NONE', #11541, 7.200000000007201528 ) ;
#9170 = DIRECTION ( 'NONE',  ( 0.000000000000000000, 0.000000000000000000, -1.000000000000000000 ) ) ;
#9171 = CARTESIAN_POINT ( 'NONE',  ( 20.00000000000000000, 0.000000000000000000, 0.000000000000000000 ) ) ;
#9172 = ORIENTED_EDGE ( 'NONE', *, *, #10349, .F. ) ;
#9173 = DIRECTION ( 'NONE',  ( 0.000000000000000000, 0.000000000000000000, -1.000000000000000000 ) ) ;
#9174 = ORIENTED_EDGE ( 'NONE', *, *, #6629, .T. ) ;
#9175 = DIRECTION ( 'NONE',  ( 0.000000000000000000, 0.000000000000000000, 1.000000000000000000 ) ) ;
#9176 = ORIENTED_EDGE ( 'NONE', *, *, #12309, .F. ) ;
#9178 = CARTESIAN_POINT ( 'NONE',  ( 45.00000000000000000, -2.534184013771451305, 4.310210132272580097 ) ) ;
#9177 = AXIS2_PLACEMENT_3D ( 'NONE', #756, #11943, #9287 ) ;
#9179 = AXIS2_PLACEMENT_3D ( 'NONE', #1988, #1054, #10424 ) ;
#9180 = EDGE_CURVE ( 'NONE', #6891, #11534, #2416, .T. ) ;
#9181 = CYLINDRICAL_SURFACE ( 'NONE', #367, 14.24900000001425227 ) ;
#9182 = ORIENTED_EDGE ( 'NONE', *, *, #9856, .T. ) ;
#9183 = CARTESIAN_POINT ( 'NONE',  ( 4.999999999999999112, 19.24938187143296275, 6.283573709965379450 ) ) ;
#9184 = AXIS2_PLACEMENT_3D ( 'NONE', #12314, #3762, #11319 ) ;
#9185 = AXIS2_PLACEMENT_3D ( 'NONE', #1687, #9083, #7192 ) ;
#9186 = ORIENTED_EDGE ( 'NONE', *, *, #1063, .T. ) ;
#9187 = AXIS2_PLACEMENT_3D ( 'NONE', #2337, #8057, #1154 ) ;
#9188 = DIRECTION ( 'NONE',  ( 0.000000000000000000, -1.000000000000000000, -1.047444401652940007E-14 ) ) ;
#9189 = EDGE_LOOP ( 'NONE', ( #6141, #11169, #1838, #6487 ) ) ;
#9190 = CARTESIAN_POINT ( 'NONE',  ( -10.00000000000000000, 0.000000000000000000, 0.000000000000000000 ) ) ;
#9191 = ORIENTED_EDGE ( 'NONE', *, *, #484, .T. ) ;
#9192 = DIRECTION ( 'NONE',  ( 0.000000000000000000, -0.4999999999999992784, 0.8660254037844389297 ) ) ;
#9193 = AXIS2_PLACEMENT_3D ( 'NONE', #8924, #7164, #338 ) ;
#9194 =( GEOMETRIC_REPRESENTATION_CONTEXT ( 3 ) GLOBAL_UNCERTAINTY_ASSIGNED_CONTEXT ( ( #9161 ) ) GLOBAL_UNIT_ASSIGNED_CONTEXT ( ( #494, #9135, #11985 ) ) REPRESENTATION_CONTEXT ( 'NONE', 'WORKASPACE' ) );
#9195 = DIRECTION ( 'NONE',  ( 0.000000000000000000, 0.000000000000000000, 1.000000000000000000 ) ) ;
#9196 = DIRECTION ( 'NONE',  ( 0.000000000000000000, 0.000000000000000000, 1.000000000000000000 ) ) ;
#9197 = FACE_OUTER_BOUND ( 'NONE', #8123, .T. ) ;
#9198 = DIRECTION ( 'NONE',  ( 0.000000000000000000, 0.000000000000000000, 1.000000000000000000 ) ) ;
#9199 = ORIENTED_EDGE ( 'NONE', *, *, #6247, .F. ) ;
#9200 = ORIENTED_EDGE ( 'NONE', *, *, #10574, .F. ) ;
#9201 = EDGE_CURVE ( 'NONE', #2664, #238, #8221, .T. ) ;
#9202 = CARTESIAN_POINT ( 'NONE',  ( -4.799999999999999822, 5.878304635907294211E-16, 0.000000000000000000 ) ) ;
#9203 = SURFACE_SIDE_STYLE ('',( #693 ) ) ;
#9204 = CIRCLE ( 'NONE', #2812, 5.000000000000000000 ) ;
#9205 = DIRECTION ( 'NONE',  ( 0.000000000000000000, 0.7900737791495477946, 0.6130117645692876316 ) ) ;
#9206 = TOROIDAL_SURFACE ( 'NONE', #3812, 7.399999999999999467, 0.1000000000000000472 ) ;
#9207 = ORIENTED_EDGE ( 'NONE', *, *, #3207, .T. ) ;
#9208 = CYLINDRICAL_SURFACE ( 'NONE', #5092, 9.600000000009600853 ) ;
#9209 = EDGE_CURVE ( 'NONE', #11506, #2800, #1031, .T. ) ;
#9210 = ORIENTED_EDGE ( 'NONE', *, *, #10825, .F. ) ;
#9211 = LINE ( 'NONE', #6461, #4036 ) ;
#9212 =( GEOMETRIC_REPRESENTATION_CONTEXT ( 3 ) GLOBAL_UNCERTAINTY_ASSIGNED_CONTEXT ( ( #6776 ) ) GLOBAL_UNIT_ASSIGNED_CONTEXT ( ( #636, #8464, #2455 ) ) REPRESENTATION_CONTEXT ( 'NONE', 'WORKASPACE' ) );
#9213 = VECTOR ( 'NONE', #6051, 1000.000000000000000 ) ;
#9214 = AXIS2_PLACEMENT_3D ( 'NONE', #3678, #730, #7497 ) ;
#9215 = CARTESIAN_POINT ( 'NONE',  ( 2.500000000000000000, 2.357898499370433054, -1.951563910473907981E-15 ) ) ;
#9216 = LINE ( 'NONE', #2512, #12133 ) ;
#9217 = DIRECTION ( 'NONE',  ( 0.000000000000000000, 0.3826834323650905589, -0.9238795325112864054 ) ) ;
#9218 = CARTESIAN_POINT ( 'NONE',  ( 4.999999999999999112, 2.791921004064247480, 22.37914155802286942 ) ) ;
#9219 = ORIENTED_EDGE ( 'NONE', *, *, #1174, .F. ) ;
#9220 = ADVANCED_FACE ( 'NONE', ( #2156 ), #293, .F. ) ;
#9221 = CARTESIAN_POINT ( 'NONE',  ( 4.999999999999999112, -14.40062958310471686, 8.872489362018137982 ) ) ;
#9222 = CARTESIAN_POINT ( 'NONE',  ( 0.000000000000000000, -1.561154383803080581, -20.18872947935932771 ) ) ;
#9223 = AXIS2_PLACEMENT_3D ( 'NONE', #1229, #6927, #10728 ) ;
#9224 = ORIENTED_EDGE ( 'NONE', *, *, #9917, .F. ) ;
#9225 = DIRECTION ( 'NONE',  ( -1.000000000000000000, 0.000000000000000000, 0.000000000000000000 ) ) ;
#9226 = VECTOR ( 'NONE', #520, 1000.000000000000000 ) ;
#9227 = ADVANCED_FACE ( 'NONE', ( #5104 ), #6160, .F. ) ;
#9228 = CONTEXT_DEPENDENT_SHAPE_REPRESENTATION ( #4969, #3246 ) ;
#9229 = CIRCLE ( 'NONE', #11014, 0.7499999999999997780 ) ;
#9230 = VERTEX_POINT ( 'NONE', #11039 ) ;
#9231 = VECTOR ( 'NONE', #411, 1000.000000000000000 ) ;
#9232 = EDGE_CURVE ( 'NONE', #10549, #3417, #2616, .T. ) ;
#9233 = SURFACE_STYLE_FILL_AREA ( #5409 ) ;
#9234 = PRESENTATION_LAYER_ASSIGNMENT (  '', '', ( #11011 ) ) ;
#9235 = CIRCLE ( 'NONE', #10414, 14.24900000001425227 ) ;
#9236 = CARTESIAN_POINT ( 'NONE',  ( 0.000000000000000000, -9.168210874537445321, -18.05452603534175893 ) ) ;
#9237 = CARTESIAN_POINT ( 'NONE',  ( -10.00000000000000000, 44.00000000000001421, 12.50000000000000000 ) ) ;
#9238 = TOROIDAL_SURFACE ( 'NONE', #3050, 2.700000000000000622, 0.2000000000000000111 ) ;
#9239 = CIRCLE ( 'NONE', #10821, 2.500000000000000444 ) ;
#9240 = DIRECTION ( 'NONE',  ( 0.000000000000000000, 0.000000000000000000, 1.000000000000000000 ) ) ;
#9241 = DIRECTION ( 'NONE',  ( 0.000000000000000000, 0.000000000000000000, 1.000000000000000000 ) ) ;
#9242 = ORIENTED_EDGE ( 'NONE', *, *, #3860, .T. ) ;
#9243 = DIRECTION ( 'NONE',  ( -1.000000000000000000, 0.000000000000000000, 0.000000000000000000 ) ) ;
#9244 = EDGE_LOOP ( 'NONE', ( #5887, #3165, #9827, #8759 ) ) ;
#9245 = FACE_OUTER_BOUND ( 'NONE', #11471, .T. ) ;
#9246 = SURFACE_SIDE_STYLE ('',( #409 ) ) ;
#9247 = ORIENTED_EDGE ( 'NONE', *, *, #1536, .T. ) ;
#9248 = CIRCLE ( 'NONE', #7249, 4.799999999999999822 ) ;
#9249 = ADVANCED_FACE ( 'NONE', ( #12030, #2471 ), #7301, .F. ) ;
#9250 = CARTESIAN_POINT ( 'NONE',  ( 20.00000000000000000, 0.000000000000000000, 12.50000000000000000 ) ) ;
#9251 = VECTOR ( 'NONE', #5965, 1000.000000000000000 ) ;
#9252 = DIRECTION ( 'NONE',  ( 0.000000000000000000, 0.000000000000000000, -1.000000000000000000 ) ) ;
#9253 = ORIENTED_EDGE ( 'NONE', *, *, #11030, .F. ) ;
#9254 = AXIS2_PLACEMENT_3D ( 'NONE', #2495, #8134, #9192 ) ;
#9255 = AXIS2_PLACEMENT_3D ( 'NONE', #4502, #4631, #2500 ) ;
#9256 = VECTOR ( 'NONE', #2719, 1000.000000000000000 ) ;
#9257 = ORIENTED_EDGE ( 'NONE', *, *, #6223, .F. ) ;
#9258 = EDGE_CURVE ( 'NONE', #7733, #11506, #5294, .T. ) ;
#9259 = VECTOR ( 'NONE', #8638, 1000.000000000000114 ) ;
#9260 = EDGE_CURVE ( 'NONE', #8560, #9354, #2226, .T. ) ;
#9261 = DIRECTION ( 'NONE',  ( 1.000000000000000000, -0.000000000000000000, -0.000000000000000000 ) ) ;
#9262 = EDGE_LOOP ( 'NONE', ( #10616, #5160, #9700, #3903 ) ) ;
#9263 = DIRECTION ( 'NONE',  ( 0.000000000000000000, -0.9238795325112906243, 0.3826834323650805114 ) ) ;
#9264 = ORIENTED_EDGE ( 'NONE', *, *, #11271, .T. ) ;
#9265 = CARTESIAN_POINT ( 'NONE',  ( 4.999999999999999112, 17.79862902732283914, -13.85025647830039119 ) ) ;
#9266 = VECTOR ( 'NONE', #9703, 1000.000000000000000 ) ;
#9267 = DIRECTION ( 'NONE',  ( 1.000000000000000000, 0.000000000000000000, 0.000000000000000000 ) ) ;
#9268 = CARTESIAN_POINT ( 'NONE',  ( 37.00000000000000711, -4.104405154062230115E-16, -2.224720805914714718E-17 ) ) ;
#9269 = DIRECTION ( 'NONE',  ( -1.000000000000000000, -1.734723475976807094E-16, 0.000000000000000000 ) ) ;
#9270 = EDGE_LOOP ( 'NONE', ( #488, #7955, #3570, #2220 ) ) ;
#9271 = ORIENTED_EDGE ( 'NONE', *, *, #78, .F. ) ;
#9272 = DIRECTION ( 'NONE',  ( 0.000000000000000000, 0.000000000000000000, -1.000000000000000000 ) ) ;
#9273 = PRESENTATION_LAYER_ASSIGNMENT (  '', '', ( #9073 ) ) ;
#9274 = CYLINDRICAL_SURFACE ( 'NONE', #12004, 7.200000000007200640 ) ;
#9275 = ORIENTED_EDGE ( 'NONE', *, *, #8369, .T. ) ;
#9276 = DIRECTION ( 'NONE',  ( -0.000000000000000000, -0.000000000000000000, -1.000000000000000000 ) ) ;
#9277 = VERTEX_POINT ( 'NONE', #9977 ) ;
#9278 = DIRECTION ( 'NONE',  ( 1.000000000000000000, 0.000000000000000000, 0.000000000000000000 ) ) ;
#9279 = PRESENTATION_LAYER_ASSIGNMENT (  '', '', ( #3887 ) ) ;
#9280 = PLANE ( 'NONE',  #3215 ) ;
#9281 = FACE_OUTER_BOUND ( 'NONE', #7848, .T. ) ;
#9282 = ADVANCED_FACE ( 'NONE', ( #3348 ), #9058, .F. ) ;
#9283 = ORIENTED_EDGE ( 'NONE', *, *, #7458, .F. ) ;
#9284 = DIRECTION ( 'NONE',  ( -1.000000000000000000, 0.000000000000000000, -0.000000000000000000 ) ) ;
#9285 = CARTESIAN_POINT ( 'NONE',  ( 15.00000000000000355, 40.00000000000000711, -1.999999999999998224 ) ) ;
#9286 = ORIENTED_EDGE ( 'NONE', *, *, #9529, .T. ) ;
#9287 = DIRECTION ( 'NONE',  ( 0.000000000000000000, -1.000000000000000000, 0.000000000000000000 ) ) ;
#9288 = CARTESIAN_POINT ( 'NONE',  ( 0.000000000000000000, 0.000000000000000000, 0.000000000000000000 ) ) ;
#9289 = ORIENTED_EDGE ( 'NONE', *, *, #9856, .F. ) ;
#9290 = CARTESIAN_POINT ( 'NONE',  ( 42.00000000000000000, 4.886001309506334600, -37.03844870997966154 ) ) ;
#9291 = CIRCLE ( 'NONE', #5684, 20.24900000002024569 ) ;
#9292 = ORIENTED_EDGE ( 'NONE', *, *, #8853, .T. ) ;
#9293 = EDGE_CURVE ( 'NONE', #4145, #8639, #3035, .T. ) ;
#9294 = CARTESIAN_POINT ( 'NONE',  ( 45.00000000000001421, 46.00000000000001421, -38.00000000000000000 ) ) ;
#9295 = CARTESIAN_POINT ( 'NONE',  ( -36.00000000000000000, 6.123233995736765296E-16, -5.000000000000000000 ) ) ;
#9296 = DIRECTION ( 'NONE',  ( 0.000000000000000000, 0.000000000000000000, 1.000000000000000000 ) ) ;
#9297 = EDGE_CURVE ( 'NONE', #10309, #9806, #1823, .T. ) ;
#9298 = CIRCLE ( 'NONE', #489, 6.975000000000000533 ) ;
#9299 = CYLINDRICAL_SURFACE ( 'NONE', #7233, 21.00000000002100009 ) ;
#9301 = ADVANCED_FACE ( 'NONE', ( #7168 ), #4404, .T. ) ;
#9300 = CARTESIAN_POINT ( 'NONE',  ( 26.00000000000000355, 0.000000000000000000, -54.50000000000000000 ) ) ;
#9302 = ORIENTED_EDGE ( 'NONE', *, *, #12172, .F. ) ;
#9303 = CARTESIAN_POINT ( 'NONE',  ( 0.000000000000000000, 0.000000000000000000, 0.000000000000000000 ) ) ;
#9304 = EDGE_LOOP ( 'NONE', ( #10967, #4133, #5499, #1915 ) ) ;
#9305 = DIRECTION ( 'NONE',  ( 0.000000000000000000, 1.000000000000000000, 0.000000000000000000 ) ) ;
#9306 = DIRECTION ( 'NONE',  ( 0.000000000000000000, 0.9242245927363030855, 0.3818493186865927203 ) ) ;
#9307 = ORIENTED_EDGE ( 'NONE', *, *, #11034, .F. ) ;
#9308 = FACE_OUTER_BOUND ( 'NONE', #5989, .T. ) ;
#9309 = VECTOR ( 'NONE', #4802, 1000.000000000000000 ) ;
#9310 = DIRECTION ( 'NONE',  ( 1.000000000000000000, 0.000000000000000000, 0.000000000000000000 ) ) ;
#9311 = ORIENTED_EDGE ( 'NONE', *, *, #8239, .T. ) ;
#9312 = CARTESIAN_POINT ( 'NONE',  ( 20.00000000000000000, 0.000000000000000000, 0.000000000000000000 ) ) ;
#9313 = EDGE_CURVE ( 'NONE', #9354, #3359, #6834, .T. ) ;
#9314 = ADVANCED_FACE ( 'NONE', ( #8926 ), #3243, .F. ) ;
#9315 = EDGE_CURVE ( 'NONE', #1890, #1765, #5622, .T. ) ;
#9316 = ORIENTED_EDGE ( 'NONE', *, *, #8114, .F. ) ;
#9317 = DIRECTION ( 'NONE',  ( -1.000000000000000000, -0.000000000000000000, 0.000000000000000000 ) ) ;
#9318 = ORIENTED_EDGE ( 'NONE', *, *, #3643, .F. ) ;
#9319 = DIRECTION ( 'NONE',  ( -1.000000000000000000, 0.000000000000000000, 0.000000000000000000 ) ) ;
#9320 = EDGE_LOOP ( 'NONE', ( #144, #9200, #8030, #8050 ) ) ;
#9321 = CYLINDRICAL_SURFACE ( 'NONE', #2562, 9.600000000009600853 ) ;
#9322 = EDGE_CURVE ( 'NONE', #7798, #2779, #10413, .T. ) ;
#9323 = ADVANCED_FACE ( 'NONE', ( #401 ), #4283, .T. ) ;
#9324 = CARTESIAN_POINT ( 'NONE',  ( 4.999999999999999112, 0.000000000000000000, 0.000000000000000000 ) ) ;
#9325 = LINE ( 'NONE', #6320, #12022 ) ;
#9326 = CARTESIAN_POINT ( 'NONE',  ( -0.1920286436967154065, 0.000000000000000000, 6.975000000000000533 ) ) ;
#9327 = VERTEX_POINT ( 'NONE', #1340 ) ;
#9328 = ORIENTED_EDGE ( 'NONE', *, *, #10083, .T. ) ;
#9329 = DIRECTION ( 'NONE',  ( 1.000000000000000000, 0.000000000000000000, 0.000000000000000000 ) ) ;
#9330 = CARTESIAN_POINT ( 'NONE',  ( 4.999999999999999112, 14.40062958310465469, 8.872489362018239234 ) ) ;
#9331 = FACE_OUTER_BOUND ( 'NONE', #5084, .T. ) ;
#9332 = VERTEX_POINT ( 'NONE', #3480 ) ;
#9333 = DIRECTION ( 'NONE',  ( 1.000000000000000000, 0.000000000000000000, -0.000000000000000000 ) ) ;
#9334 = ADVANCED_FACE ( 'NONE', ( #341 ), #9437, .F. ) ;
#9335 = CARTESIAN_POINT ( 'NONE',  ( 0.000000000000000000, -13.09267581720862950, -5.622796541391702263 ) ) ;
#9336 = LINE ( 'NONE', #6210, #11259 ) ;
#9337 = VERTEX_POINT ( 'NONE', #4221 ) ;
#9338 = FACE_OUTER_BOUND ( 'NONE', #850, .T. ) ;
#9339 = DIRECTION ( 'NONE',  ( 0.000000000000000000, 0.7071067811865439090, 0.7071067811865511255 ) ) ;
#9340 = EDGE_LOOP ( 'NONE', ( #4913, #2530, #9118, #7830, #3482, #2293 ) ) ;
#9341 = DIRECTION ( 'NONE',  ( -1.000000000000000000, 0.000000000000000000, -0.000000000000000000 ) ) ;
#9342 = CYLINDRICAL_SURFACE ( 'NONE', #5428, 6.975000000000000533 ) ;
#9343 = VERTEX_POINT ( 'NONE', #11845 ) ;
#9344 = DIRECTION ( 'NONE',  ( -1.000000000000000000, -0.000000000000000000, -0.000000000000000000 ) ) ;
#9345 = ORIENTED_EDGE ( 'NONE', *, *, #63, .T. ) ;
#9346 = DIRECTION ( 'NONE',  ( -1.000000000000000000, -0.000000000000000000, -0.000000000000000000 ) ) ;
#9347 = DIRECTION ( 'NONE',  ( -0.000000000000000000, -1.000000000000000000, -0.000000000000000000 ) ) ;
#9348 = DIRECTION ( 'NONE',  ( 0.000000000000000000, 0.000000000000000000, -1.000000000000000000 ) ) ;
#9349 = CARTESIAN_POINT ( 'NONE',  ( 42.00000000000000000, 4.769696007084728073, 1.500000000000000444 ) ) ;
#9350 = DIRECTION ( 'NONE',  ( -1.000000000000000000, -0.000000000000000000, -0.000000000000000000 ) ) ;
#9351 = EDGE_LOOP ( 'NONE', ( #1412, #1793 ) ) ;
#9352 = ORIENTED_EDGE ( 'NONE', *, *, #8677, .T. ) ;
#9353 = DIRECTION ( 'NONE',  ( 0.000000000000000000, 0.000000000000000000, 1.000000000000000000 ) ) ;
#9354 = VERTEX_POINT ( 'NONE', #2772 ) ;
#9355 = EDGE_CURVE ( 'NONE', #5401, #9980, #3049, .T. ) ;
#9356 = APPLICATION_PROTOCOL_DEFINITION ( 'draft international standard', 'automotive_design', 1998, #3227 ) ;
#9357 = ORIENTED_EDGE ( 'NONE', *, *, #4457, .T. ) ;
#9358 = CARTESIAN_POINT ( 'NONE',  ( -15.00000000000000000, 40.00000000000000711, -2.000000000000000000 ) ) ;
#9359 = ADVANCED_FACE ( 'NONE', ( #2587 ), #9299, .T. ) ;
#9360 = CARTESIAN_POINT ( 'NONE',  ( -36.00000000000000000, 0.000000000000000000, -5.999999999999999112 ) ) ;
#9361 = CIRCLE ( 'NONE', #3770, 21.00000000002100009 ) ;
#9362 = ORIENTED_EDGE ( 'NONE', *, *, #4858, .T. ) ;
#9363 = CARTESIAN_POINT ( 'NONE',  ( 1.399999999999999689, 0.000000000000000000, 0.000000000000000000 ) ) ;
#9364 = DIRECTION ( 'NONE',  ( 1.000000000000000000, -0.000000000000000000, -0.000000000000000000 ) ) ;
#9365 = ORIENTED_EDGE ( 'NONE', *, *, #914, .F. ) ;
#9366 = DIRECTION ( 'NONE',  ( 0.000000000000000000, 0.000000000000000000, 1.000000000000000000 ) ) ;
#9367 = AXIS2_PLACEMENT_3D ( 'NONE', #5727, #8549, #7494 ) ;
#9368 = ORIENTED_EDGE ( 'NONE', *, *, #7157, .F. ) ;
#9369 = EDGE_CURVE ( 'NONE', #7721, #6749, #11616, .T. ) ;
#9370 =( NAMED_UNIT ( * ) SI_UNIT ( $, .STERADIAN. ) SOLID_ANGLE_UNIT ( ) );
#9371 = DIRECTION ( 'NONE',  ( -1.000000000000000000, -0.000000000000000000, -0.000000000000000000 ) ) ;
#9372 = EDGE_CURVE ( 'NONE', #5533, #11913, #9043, .T. ) ;
#9374 = ORIENTED_EDGE ( 'NONE', *, *, #9745, .T. ) ;
#9373 = ADVANCED_FACE ( 'NONE', ( #11152 ), #659, .F. ) ;
#9375 = FACE_OUTER_BOUND ( 'NONE', #11074, .T. ) ;
#9376 = EDGE_CURVE ( 'NONE', #7805, #6322, #10332, .T. ) ;
#9377 = CIRCLE ( 'NONE', #8784, 7.200000000007202416 ) ;
#9378 = AXIS2_PLACEMENT_3D ( 'NONE', #6693, #9436, #12230 ) ;
#9379 = DIRECTION ( 'NONE',  ( -1.000000000000000000, -0.000000000000000000, -0.000000000000000000 ) ) ;
#9380 = AXIS2_PLACEMENT_3D ( 'NONE', #1661, #2523, #6345 ) ;
#9381 = DIRECTION ( 'NONE',  ( -1.000000000000000000, -3.903127820947815962E-18, 0.000000000000000000 ) ) ;
#9382 = CARTESIAN_POINT ( 'NONE',  ( -20.00000000000000000, 0.000000000000000000, 25.00000000000000000 ) ) ;
#9383 = VERTEX_POINT ( 'NONE', #10279 ) ;
#9384 = VERTEX_POINT ( 'NONE', #1851 ) ;
#9385 = LINE ( 'NONE', #6567, #1475 ) ;
#9386 = EDGE_CURVE ( 'NONE', #8321, #4719, #11412, .T. ) ;
#9387 = LINE ( 'NONE', #5562, #6639 ) ;
#9388 = CARTESIAN_POINT ( 'NONE',  ( 4.999999999999999112, 14.46592441914964766, 15.22291137398927141 ) ) ;
#9389 = AXIS2_PLACEMENT_3D ( 'NONE', #3825, #12249, #11498 ) ;
#9390 = EDGE_LOOP ( 'NONE', ( #9145, #9821, #10160, #7947 ) ) ;
#9391 = DIRECTION ( 'NONE',  ( 0.000000000000000000, 0.000000000000000000, 1.000000000000000000 ) ) ;
#9392 = VECTOR ( 'NONE', #6729, 1000.000000000000000 ) ;
#9393 = CARTESIAN_POINT ( 'NONE',  ( 26.00000000000000355, 0.000000000000000000, -41.99999999999999289 ) ) ;
#9394 = CARTESIAN_POINT ( 'NONE',  ( 4.999999999999999112, 16.90755573046745397, 0.4834863907628708102 ) ) ;
#9395 = EDGE_LOOP ( 'NONE', ( #4397, #10898, #7022, #2891 ) ) ;
#9396 = AXIS2_PLACEMENT_3D ( 'NONE', #7181, #4116, #2169 ) ;
#9397 = DIRECTION ( 'NONE',  ( -1.000000000000000000, 0.000000000000000000, 0.000000000000000000 ) ) ;
#9398 = CARTESIAN_POINT ( 'NONE',  ( 0.000000000000000000, -14.14998813191271054, 1.676853263447836806 ) ) ;
#9399 = ORIENTED_EDGE ( 'NONE', *, *, #5022, .F. ) ;
#9400 = CARTESIAN_POINT ( 'NONE',  ( 0.000000000000000000, -22.83261415639512748, 14.41081992069302053 ) ) ;
#9401 = EDGE_CURVE ( 'NONE', #9928, #3605, #8832, .T. ) ;
#9402 = DIRECTION ( 'NONE',  ( 0.000000000000000000, -1.224646799147353454E-16, 1.000000000000000000 ) ) ;
#9403 = EDGE_CURVE ( 'NONE', #9620, #7019, #11217, .T. ) ;
#9404 = EDGE_LOOP ( 'NONE', ( #2850, #9191, #9992, #10693 ) ) ;
#9405 = CARTESIAN_POINT ( 'NONE',  ( 0.000000000000000000, -1.676853263447787068, -14.14998813191271410 ) ) ;
#9406 = UNCERTAINTY_MEASURE_WITH_UNIT (LENGTH_MEASURE( 1.000000000000000082E-05 ), #71, 'distance_accuracy_value', 'NONE');
#9407 = ORIENTED_EDGE ( 'NONE', *, *, #8213, .T. ) ;
#9408 = AXIS2_PLACEMENT_3D ( 'NONE', #10128, #2547, #1796 ) ;
#9409 = DIRECTION ( 'NONE',  ( 0.000000000000000000, 0.000000000000000000, 1.000000000000000000 ) ) ;
#9410 = CARTESIAN_POINT ( 'NONE',  ( 65.79898987322334847, 5.744562646538041051, -38.00000000000000000 ) ) ;
#9411 = DIRECTION ( 'NONE',  ( -1.000000000000000000, -0.000000000000000000, -0.000000000000000000 ) ) ;
#9412 = CARTESIAN_POINT ( 'NONE',  ( 5.000000000000000000, 0.000000000000000000, 1.500000000000000000 ) ) ;
#9413 = AXIS2_PLACEMENT_3D ( 'NONE', #7526, #11320, #6723 ) ;
#9414 = VERTEX_POINT ( 'NONE', #1664 ) ;
#9415 = EDGE_LOOP ( 'NONE', ( #1628, #12122, #10388, #6366 ) ) ;
#9416 = AXIS2_PLACEMENT_3D ( 'NONE', #3301, #4284, #7169 ) ;
#9417 = DIRECTION ( 'NONE',  ( -1.000000000000000000, -0.000000000000000000, -0.000000000000000000 ) ) ;
#9418 = CIRCLE ( 'NONE', #6222, 5.000000000000000000 ) ;
#9419 = ORIENTED_EDGE ( 'NONE', *, *, #5768, .F. ) ;
#9420 = DIRECTION ( 'NONE',  ( -1.000000000000000000, 0.000000000000000000, 0.000000000000000000 ) ) ;
#9421 = CARTESIAN_POINT ( 'NONE',  ( 51.00000000000000000, 0.000000000000000000, -41.99999999999999289 ) ) ;
#9422 = ORIENTED_EDGE ( 'NONE', *, *, #2353, .T. ) ;
#9423 = LINE ( 'NONE', #4018, #5216 ) ;
#9424 = CARTESIAN_POINT ( 'NONE',  ( 4.999999999999999112, 0.000000000000000000, 0.000000000000000000 ) ) ;
#9425 = CIRCLE ( 'NONE', #11808, 6.080745460913608902 ) ;
#9426 = AXIS2_PLACEMENT_3D ( 'NONE', #1511, #3208, #5270 ) ;
#9427 = AXIS2_PLACEMENT_3D ( 'NONE', #7415, #769, #11218 ) ;
#9428 = VERTEX_POINT ( 'NONE', #9349 ) ;
#9429 = VECTOR ( 'NONE', #6142, 1000.000000000000000 ) ;
#9430 = VERTEX_POINT ( 'NONE', #10223 ) ;
#9431 = CARTESIAN_POINT ( 'NONE',  ( 37.00000000000000711, 6.799999999999998046, -1.500000000000000000 ) ) ;
#9432 = DIRECTION ( 'NONE',  ( 2.817067928751547788E-17, 0.6371047110838219396, -0.7707772616747329275 ) ) ;
#9433 = DIRECTION ( 'NONE',  ( 0.000000000000000000, 0.000000000000000000, -1.000000000000000000 ) ) ;
#9434 = EDGE_CURVE ( 'NONE', #10148, #6613, #6348, .T. ) ;
#9435 = ORIENTED_EDGE ( 'NONE', *, *, #6702, .T. ) ;
#9436 = DIRECTION ( 'NONE',  ( -1.000000000000000000, 0.000000000000000000, -0.000000000000000000 ) ) ;
#9437 = CONICAL_SURFACE ( 'NONE', #4229, 2.041999999999999815, 1.047197551196591858 ) ;
#9438 = ORIENTED_EDGE ( 'NONE', *, *, #12250, .T. ) ;
#9439 = CIRCLE ( 'NONE', #5041, 1.199999999999999956 ) ;
#9440 =( NAMED_UNIT ( * ) SI_UNIT ( $, .STERADIAN. ) SOLID_ANGLE_UNIT ( ) );
#9441 = AXIS2_PLACEMENT_3D ( 'NONE', #210, #5205, #4030 ) ;
#9442 = DIRECTION ( 'NONE',  ( 0.000000000000000000, 0.000000000000000000, 1.000000000000000000 ) ) ;
#9443 = ORIENTED_EDGE ( 'NONE', *, *, #8714, .F. ) ;
#9444 = LINE ( 'NONE', #5809, #10553 ) ;
#9445 = AXIS2_PLACEMENT_3D ( 'NONE', #3670, #2723, #4599 ) ;
#9446 = CIRCLE ( 'NONE', #5245, 4.000000000000000000 ) ;
#9447 = CIRCLE ( 'NONE', #1822, 2.700000000000000178 ) ;
#9448 = DIRECTION ( 'NONE',  ( -1.000000000000000000, -0.000000000000000000, 0.000000000000000000 ) ) ;
#9449 = EDGE_CURVE ( 'NONE', #7924, #4331, #10158, .T. ) ;
#9450 = VECTOR ( 'NONE', #4746, 1000.000000000000000 ) ;
#9451 = ADVANCED_FACE ( 'NONE', ( #6533 ), #5531, .F. ) ;
#9452 = PLANE ( 'NONE',  #7778 ) ;
#9453 = CARTESIAN_POINT ( 'NONE',  ( 0.000000000000000000, 0.000000000000000000, 0.000000000000000000 ) ) ;
#9454 = EDGE_CURVE ( 'NONE', #1842, #4309, #4717, .T. ) ;
#9455 = ORIENTED_EDGE ( 'NONE', *, *, #11725, .F. ) ;
#9456 = VERTEX_POINT ( 'NONE', #8537 ) ;
#9457 = DIRECTION ( 'NONE',  ( 1.000000000000000000, 0.000000000000000000, 0.000000000000000000 ) ) ;
#9458 = ADVANCED_BREP_SHAPE_REPRESENTATION ( '', ( #259, #6056 ), #8623 ) ;
#9459 = DIRECTION ( 'NONE',  ( -1.000000000000000000, -0.000000000000000000, -0.000000000000000000 ) ) ;
#9460 = FACE_OUTER_BOUND ( 'NONE', #6451, .T. ) ;
#9461 = AXIS2_PLACEMENT_3D ( 'NONE', #5815, #122, #11248 ) ;
#9462 = ORIENTED_EDGE ( 'NONE', *, *, #9829, .T. ) ;
#9463 = CARTESIAN_POINT ( 'NONE',  ( 4.999999999999999112, 15.37949036966230132, -13.17168466712912434 ) ) ;
#9464 = SURFACE_STYLE_USAGE ( .BOTH. , #11314 ) ;
#9465 = DIRECTION ( 'NONE',  ( 0.000000000000000000, -0.7091011189803927417, 0.7051068025914618564 ) ) ;
#9466 = AXIS2_PLACEMENT_3D ( 'NONE', #8822, #124, #9885 ) ;
#9467 = ORIENTED_EDGE ( 'NONE', *, *, #2698, .T. ) ;
#9468 = DIRECTION ( 'NONE',  ( -1.000000000000000000, 0.000000000000000000, 0.000000000000000000 ) ) ;
#9469 = CYLINDRICAL_SURFACE ( 'NONE', #5844, 4.800000000000000711 ) ;
#9470 = EDGE_CURVE ( 'NONE', #11850, #7774, #6038, .T. ) ;
#9471 = ORIENTED_EDGE ( 'NONE', *, *, #135, .T. ) ;
#9472 = CARTESIAN_POINT ( 'NONE',  ( 26.00000000000000355, 0.000000000000000000, -41.99999999999999289 ) ) ;
#9473 = DIRECTION ( 'NONE',  ( -0.000000000000000000, -0.000000000000000000, -1.000000000000000000 ) ) ;
#9474 = VERTEX_POINT ( 'NONE', #3597 ) ;
#9475 = DIRECTION ( 'NONE',  ( -1.000000000000000000, 0.000000000000000000, 0.000000000000000000 ) ) ;
#9476 = ORIENTED_EDGE ( 'NONE', *, *, #9133, .F. ) ;
#9477 = CIRCLE ( 'NONE', #5276, 6.975000000000000533 ) ;
#9478 = EDGE_CURVE ( 'NONE', #3694, #611, #836, .T. ) ;
#9479 = EDGE_CURVE ( 'NONE', #7148, #1686, #2659, .T. ) ;
#9480 = CARTESIAN_POINT ( 'NONE',  ( 0.000000000000000000, -14.40062958310471686, 8.872489362018137982 ) ) ;
#9481 = DIRECTION ( 'NONE',  ( 0.000000000000000000, 0.8772744497699203059, 0.4799891038147465760 ) ) ;
#9482 = DIRECTION ( 'NONE',  ( -1.000000000000000000, -0.000000000000000000, -0.000000000000000000 ) ) ;
#9483 = DIRECTION ( 'NONE',  ( -1.000000000000000000, 0.000000000000000000, -0.000000000000000000 ) ) ;
#9484 = ORIENTED_EDGE ( 'NONE', *, *, #7095, .F. ) ;
#9485 = VERTEX_POINT ( 'NONE', #8481 ) ;
#9486 = CARTESIAN_POINT ( 'NONE',  ( 0.000000000000000000, 0.000000000000000000, 0.000000000000000000 ) ) ;
#9487 = EDGE_LOOP ( 'NONE', ( #1220, #8725, #11765, #8341 ) ) ;
#9488 = DIRECTION ( 'NONE',  ( 0.000000000000000000, 0.000000000000000000, 1.000000000000000000 ) ) ;
#9489 = SHAPE_DEFINITION_REPRESENTATION ( #5829, #10563 ) ;
#9490 = VERTEX_POINT ( 'NONE', #11329 ) ;
#9491 = DIRECTION ( 'NONE',  ( 0.000000000000000000, 0.000000000000000000, 1.000000000000000000 ) ) ;
#9492 = DIRECTION ( 'NONE',  ( 1.000000000000000000, 0.000000000000000000, 0.000000000000000000 ) ) ;
#9493 = CIRCLE ( 'NONE', #7897, 7.200000000007200640 ) ;
#9494 = ORIENTED_EDGE ( 'NONE', *, *, #1719, .T. ) ;
#9495 = ORIENTED_EDGE ( 'NONE', *, *, #6033, .T. ) ;
#9496 = CARTESIAN_POINT ( 'NONE',  ( 0.000000000000000000, 0.5192545390863916310, -1.000000000000000000 ) ) ;
#9497 = PLANE ( 'NONE',  #7028 ) ;
#9498 = CARTESIAN_POINT ( 'NONE',  ( 4.999999999999999112, -8.527191590520994069, -11.41582255376081889 ) ) ;
#9499 = ORIENTED_EDGE ( 'NONE', *, *, #10914, .F. ) ;
#9500 = CARTESIAN_POINT ( 'NONE',  ( 4.999999999999999112, 0.000000000000000000, 0.000000000000000000 ) ) ;
#9501 = ORIENTED_EDGE ( 'NONE', *, *, #6760, .T. ) ;
#9502 = AXIS2_PLACEMENT_3D ( 'NONE', #4495, #429, #7128 ) ;
#9503 = ORIENTED_EDGE ( 'NONE', *, *, #3643, .T. ) ;
#9504 = DIRECTION ( 'NONE',  ( -1.000000000000000000, 0.000000000000000000, -0.000000000000000000 ) ) ;
#9505 = VERTEX_POINT ( 'NONE', #11651 ) ;
#9506 = DIRECTION ( 'NONE',  ( 1.000000000000000000, 0.000000000000000000, 0.000000000000000000 ) ) ;
#9507 = CARTESIAN_POINT ( 'NONE',  ( 36.00000000000000711, -3.545505594901966262, -38.47446598704267728 ) ) ;
#9508 = CARTESIAN_POINT ( 'NONE',  ( 4.999999999999999112, -8.872489362018288972, 14.40062958310462271 ) ) ;
#9509 = DIRECTION ( 'NONE',  ( 0.000000000000000000, -1.000000000000000000, 0.000000000000000000 ) ) ;
#9510 = ORIENTED_EDGE ( 'NONE', *, *, #495, .F. ) ;
#9511 = ORIENTED_EDGE ( 'NONE', *, *, #11488, .T. ) ;
#9512 = CARTESIAN_POINT ( 'NONE',  ( 37.00000000000000711, -3.403685371105885427, -38.61548734756097190 ) ) ;
#9513 = DIRECTION ( 'NONE',  ( 0.000000000000000000, 0.000000000000000000, 1.000000000000000000 ) ) ;
#9514 = CARTESIAN_POINT ( 'NONE',  ( 0.000000000000000000, 4.641444688392526779E-16, 3.790027207537782772 ) ) ;
#9515 = EDGE_CURVE ( 'NONE', #6632, #3914, #7673, .T. ) ;
#9516 = ORIENTED_EDGE ( 'NONE', *, *, #3005, .F. ) ;
#9517 = DIRECTION ( 'NONE',  ( 0.000000000000000000, 0.6828850436591804574, 0.7305258497456468270 ) ) ;
#9518 = EDGE_CURVE ( 'NONE', #6756, #9537, #6848, .T. ) ;
#9519 = DIRECTION ( 'NONE',  ( -1.000000000000000000, -0.000000000000000000, -0.000000000000000000 ) ) ;
#9520 = CARTESIAN_POINT ( 'NONE',  ( 0.2500000000000002220, 0.000000000000000000, 4.250000000000000000 ) ) ;
#9521 = CARTESIAN_POINT ( 'NONE',  ( -15.00000000000000000, 44.00000000000001421, 2.149999999999999023 ) ) ;
#9522 = ORIENTED_EDGE ( 'NONE', *, *, #2879, .T. ) ;
#9523 = CARTESIAN_POINT ( 'NONE',  ( -2.595115354961444076, -7.673029147243174641, 0.000000000000000000 ) ) ;
#9524 = FACE_OUTER_BOUND ( 'NONE', #7280, .T. ) ;
#9525 = ORIENTED_EDGE ( 'NONE', *, *, #10193, .T. ) ;
#9526 = DIRECTION ( 'NONE',  ( 0.000000000000000000, 0.3826834323650840641, 0.9238795325112890700 ) ) ;
#9527 = UNCERTAINTY_MEASURE_WITH_UNIT (LENGTH_MEASURE( 1.000000000000000082E-05 ), #1597, 'distance_accuracy_value', 'NONE');
#9528 = VERTEX_POINT ( 'NONE', #1029 ) ;
#9529 = EDGE_CURVE ( 'NONE', #7970, #12234, #11517, .T. ) ;
#9530 = EDGE_CURVE ( 'NONE', #5710, #702, #2233, .T. ) ;
#9531 = EDGE_CURVE ( 'NONE', #8473, #11449, #4847, .T. ) ;
#9532 = DIRECTION ( 'NONE',  ( -1.000000000000000000, 0.000000000000000000, 0.000000000000000000 ) ) ;
#9533 = FACE_OUTER_BOUND ( 'NONE', #101, .T. ) ;
#9534 = DIRECTION ( 'NONE',  ( 0.000000000000000000, 0.8660254037844398178, -0.4999999999999980016 ) ) ;
#9535 = CARTESIAN_POINT ( 'NONE',  ( 0.000000000000000000, 0.000000000000000000, 0.000000000000000000 ) ) ;
#9536 = DIRECTION ( 'NONE',  ( 1.000000000000000000, 0.000000000000000000, 0.000000000000000000 ) ) ;
#9537 = VERTEX_POINT ( 'NONE', #3910 ) ;
#9538 = EDGE_LOOP ( 'NONE', ( #9002, #5304, #7201, #12218 ) ) ;
#9539 =( NAMED_UNIT ( * ) SI_UNIT ( $, .STERADIAN. ) SOLID_ANGLE_UNIT ( ) );
#9540 = ORIENTED_EDGE ( 'NONE', *, *, #11134, .F. ) ;
#9541 = DIRECTION ( 'NONE',  ( 0.000000000000000000, 0.000000000000000000, -1.000000000000000000 ) ) ;
#9542 = UNCERTAINTY_MEASURE_WITH_UNIT (LENGTH_MEASURE( 1.000000000000000082E-05 ), #10397, 'distance_accuracy_value', 'NONE');
#9543 = APPLICATION_PROTOCOL_DEFINITION ( 'draft international standard', 'automotive_design', 1998, #7131 ) ;
#9544 = EDGE_CURVE ( 'NONE', #8252, #11850, #10663, .T. ) ;
#9545 = ORIENTED_EDGE ( 'NONE', *, *, #9479, .F. ) ;
#9546 = DIRECTION ( 'NONE',  ( 0.000000000000000000, 0.000000000000000000, 1.000000000000000000 ) ) ;
#9547 = ORIENTED_EDGE ( 'NONE', *, *, #9989, .T. ) ;
#9548 = EDGE_LOOP ( 'NONE', ( #2279, #6711, #2753, #9362 ) ) ;
#9549 = CARTESIAN_POINT ( 'NONE',  ( 4.999999999999999112, 0.000000000000000000, 0.000000000000000000 ) ) ;
#9550 = DIRECTION ( 'NONE',  ( -1.000000000000000000, 0.000000000000000000, -0.000000000000000000 ) ) ;
#9551 = LINE ( 'NONE', #7741, #828 ) ;
#9552 = PLANE ( 'NONE',  #2418 ) ;
#9553 = ORIENTED_EDGE ( 'NONE', *, *, #7609, .F. ) ;
#9554 = CARTESIAN_POINT ( 'NONE',  ( 0.000000000000000000, 14.41081992069310047, 22.83261415639507774 ) ) ;
#9555 = ORIENTED_EDGE ( 'NONE', *, *, #11189, .T. ) ;
#9556 = EDGE_CURVE ( 'NONE', #8570, #9112, #9425, .T. ) ;
#9557 = ORIENTED_EDGE ( 'NONE', *, *, #324, .T. ) ;
#9558 = DIRECTION ( 'NONE',  ( 0.000000000000000000, 0.000000000000000000, 1.000000000000000000 ) ) ;
#9559 = ORIENTED_EDGE ( 'NONE', *, *, #1732, .T. ) ;
#9560 = CARTESIAN_POINT ( 'NONE',  ( 4.999999999999999112, 0.000000000000000000, 0.000000000000000000 ) ) ;
#9561 = VECTOR ( 'NONE', #5715, 1000.000000000000000 ) ;
#9562 = LINE ( 'NONE', #8696, #11972 ) ;
#9563 = AXIS2_PLACEMENT_3D ( 'NONE', #3879, #4804, #2801 ) ;
#9564 = VECTOR ( 'NONE', #6941, 1000.000000000000000 ) ;
#9565 = CARTESIAN_POINT ( 'NONE',  ( 0.3697398607305836249, -0.6000000000000000888, 3.517354947232271378 ) ) ;
#9566 = FACE_OUTER_BOUND ( 'NONE', #3928, .T. ) ;
#9567 = ORIENTED_EDGE ( 'NONE', *, *, #1130, .T. ) ;
#9568 = DIRECTION ( 'NONE',  ( 4.000869187770762975E-18, 0.8386705679454229401, 0.5446390350150287496 ) ) ;
#9569 = CARTESIAN_POINT ( 'NONE',  ( 33.00000000000000000, 0.000000000000000000, 0.000000000000000000 ) ) ;
#9570 = PLANE ( 'NONE',  #9693 ) ;
#9571 = ORIENTED_EDGE ( 'NONE', *, *, #1326, .F. ) ;
#9572 = CARTESIAN_POINT ( 'NONE',  ( 46.00000000000000000, 4.817162211711311315, -40.66024322130446222 ) ) ;
#9573 = AXIS2_PLACEMENT_3D ( 'NONE', #2573, #10268, #4389 ) ;
#9574 = TOROIDAL_SURFACE ( 'NONE', #11354, 6.250000000000000000, 0.7500000000000000000 ) ;
#9575 = CLOSED_SHELL ( 'NONE', ( #11410, #2182, #7463, #4939, #336, #6246, #12327, #3173, #11792, #5238, #7867, #7094, #11344, #5390, #9897, #7186, #1485, #7410, #663, #9451, #10215, #10229, #2354, #3554, #1437, #10455, #6780, #12247, #2935, #2552, #3354, #10267, #12089, #7269, #5037, #7541, #2173, #5567, #9708, #1869 ) ) ;
#9576 = DIRECTION ( 'NONE',  ( 1.000000000000000000, 1.734723475976807094E-16, 0.000000000000000000 ) ) ;
#9577 = FACE_OUTER_BOUND ( 'NONE', #10689, .T. ) ;
#9578 = EDGE_CURVE ( 'NONE', #3907, #102, #12204, .T. ) ;
#9579 = DIRECTION ( 'NONE',  ( 0.000000000000000000, 0.000000000000000000, -1.000000000000000000 ) ) ;
#9580 = CARTESIAN_POINT ( 'NONE',  ( 0.000000000000000000, 22.37914155802281257, 2.791921004064645384 ) ) ;
#9581 = CIRCLE ( 'NONE', #4182, 5.000000000000004441 ) ;
#9582 = CIRCLE ( 'NONE', #3559, 7.000000000000000000 ) ;
#9583 = ORIENTED_EDGE ( 'NONE', *, *, #4539, .F. ) ;
#9584 = EDGE_CURVE ( 'NONE', #9031, #403, #6860, .T. ) ;
#9585 = DIRECTION ( 'NONE',  ( -1.000000000000000000, -0.000000000000000000, 0.000000000000000000 ) ) ;
#9586 = DIRECTION ( 'NONE',  ( 1.000000000000000000, -0.000000000000000000, -0.000000000000000000 ) ) ;
#9587 = VERTEX_POINT ( 'NONE', #10469 ) ;
#9588 = DIRECTION ( 'NONE',  ( 0.000000000000000000, 0.8660254037844362651, 0.5000000000000038858 ) ) ;
#9589 = ORIENTED_EDGE ( 'NONE', *, *, #790, .T. ) ;
#9590 = VECTOR ( 'NONE', #9347, 1000.000000000000000 ) ;
#9591 = DIRECTION ( 'NONE',  ( 0.000000000000000000, 0.000000000000000000, 1.000000000000000000 ) ) ;
#9592 = CIRCLE ( 'NONE', #613, 6.750000000000000000 ) ;
#9593 = CARTESIAN_POINT ( 'NONE',  ( 65.79898987322334847, 5.000000000000004441, -41.99999999999998579 ) ) ;
#9594 = CARTESIAN_POINT ( 'NONE',  ( 0.000000000000000000, 0.000000000000000000, 0.000000000000000000 ) ) ;
#9595 = EDGE_CURVE ( 'NONE', #3450, #4147, #5027, .T. ) ;
#9596 = DIRECTION ( 'NONE',  ( 1.000000000000000000, 0.000000000000000000, 0.000000000000000000 ) ) ;
#9597 = DIRECTION ( 'NONE',  ( 0.000000000000000000, 0.7071067811865439090, 0.7071067811865512365 ) ) ;
#9598 = VERTEX_POINT ( 'NONE', #5914 ) ;
#9600 = ADVANCED_FACE ( 'NONE', ( #10714 ), #9669, .T. ) ;
#9599 = ORIENTED_EDGE ( 'NONE', *, *, #10676, .T. ) ;
#9601 = ADVANCED_FACE ( 'NONE', ( #2145 ), #5025, .T. ) ;
#9602 = VECTOR ( 'NONE', #1385, 1000.000000000000000 ) ;
#9603 = ORIENTED_EDGE ( 'NONE', *, *, #7384, .F. ) ;
#9604 = CARTESIAN_POINT ( 'NONE',  ( 37.00000000000000711, 1.456773409934505593E-31, -41.99999999999998579 ) ) ;
#9605 = APPLICATION_PROTOCOL_DEFINITION ( 'draft international standard', 'automotive_design', 1998, #493 ) ;
#9606 = VECTOR ( 'NONE', #11634, 1000.000000000000000 ) ;
#9607 = ORIENTED_EDGE ( 'NONE', *, *, #884, .F. ) ;
#9608 = VECTOR ( 'NONE', #657, 1000.000000000000000 ) ;
#9609 = EDGE_LOOP ( 'NONE', ( #12091, #8494, #9419, #9735 ) ) ;
#9610 = AXIS2_PLACEMENT_3D ( 'NONE', #1, #888, #3010 ) ;
#9611 = VERTEX_POINT ( 'NONE', #11461 ) ;
#9612 = AXIS2_PLACEMENT_3D ( 'NONE', #1392, #2462, #10099 ) ;
#9613 = DIRECTION ( 'NONE',  ( -1.000000000000000000, -0.000000000000000000, -0.000000000000000000 ) ) ;
#9614 = CARTESIAN_POINT ( 'NONE',  ( 0.000000000000000000, 16.90755573046746107, -0.4834863907626340551 ) ) ;
#9615 = VECTOR ( 'NONE', #4734, 1000.000000000000000 ) ;
#9616 = CIRCLE ( 'NONE', #4212, 27.00000000002699707 ) ;
#9617 = VECTOR ( 'NONE', #11047, 1000.000000000000000 ) ;
#9618 = CARTESIAN_POINT ( 'NONE',  ( 51.00000000000000000, -3.499999999999998668, -38.49999999999998579 ) ) ;
#9619 = FACE_OUTER_BOUND ( 'NONE', #7040, .T. ) ;
#9620 = VERTEX_POINT ( 'NONE', #11396 ) ;
#9621 = DIRECTION ( 'NONE',  ( 1.000000000000000000, 0.000000000000000000, 0.000000000000000000 ) ) ;
#9622 = EDGE_CURVE ( 'NONE', #4193, #10979, #2911, .T. ) ;
#9623 = ORIENTED_EDGE ( 'NONE', *, *, #1731, .F. ) ;
#9624 = ORIENTED_EDGE ( 'NONE', *, *, #11488, .F. ) ;
#9625 = COLOUR_RGB ( '',0.8941176470588234615, 0.8941176470588234615, 0.8941176470588234615 ) ;
#9626 = AXIS2_PLACEMENT_3D ( 'NONE', #10998, #6549, #10295 ) ;
#9627 = CARTESIAN_POINT ( 'NONE',  ( 0.000000000000000000, -16.90755573046746463, 0.4834863907625160939 ) ) ;
#9628 = VECTOR ( 'NONE', #11876, 1000.000000000000114 ) ;
#9629 = PRODUCT_DEFINITION_SHAPE ( 'NONE', 'NONE',  #11287 ) ;
#9630 = CIRCLE ( 'NONE', #7630, 3.885863436426969297 ) ;
#9631 = ORIENTED_EDGE ( 'NONE', *, *, #6813, .F. ) ;
#9632 = PLANE ( 'NONE',  #11738 ) ;
#9633 = AXIS2_PLACEMENT_3D ( 'NONE', #1271, #10838, #8851 ) ;
#9634 = FACE_OUTER_BOUND ( 'NONE', #3498, .T. ) ;
#9635 = EDGE_CURVE ( 'NONE', #12046, #2589, #3431, .T. ) ;
#9636 = EDGE_CURVE ( 'NONE', #3807, #1747, #5716, .T. ) ;
#9637 = COLOUR_RGB ( '',1.000000000000000000, 0.9490196078431372140, 0.9098039215686274384 ) ;
#9638 = AXIS2_PLACEMENT_3D ( 'NONE', #9535, #10525, #5778 ) ;
#9639 = AXIS2_PLACEMENT_3D ( 'NONE', #806, #5382, #8384 ) ;
#9640 = AXIS2_PLACEMENT_3D ( 'NONE', #12071, #6467, #1705 ) ;
#9641 = FACE_OUTER_BOUND ( 'NONE', #10095, .T. ) ;
#9642 = DIRECTION ( 'NONE',  ( 1.000000000000000000, 0.000000000000000000, 0.000000000000000000 ) ) ;
#9643 = VERTEX_POINT ( 'NONE', #5854 ) ;
#9644 = CARTESIAN_POINT ( 'NONE',  ( 46.00000000000000000, 3.500000000000001332, -45.49999999999998579 ) ) ;
#9645 = DIRECTION ( 'NONE',  ( -1.000000000000000000, -0.000000000000000000, -0.000000000000000000 ) ) ;
#9646 = CYLINDRICAL_SURFACE ( 'NONE', #11272, 5.000000000000000000 ) ;
#9647 = ORIENTED_EDGE ( 'NONE', *, *, #3294, .T. ) ;
#9648 = DIRECTION ( 'NONE',  ( -1.000000000000000000, 0.000000000000000000, -0.000000000000000000 ) ) ;
#9649 = PRODUCT_DEFINITION_FORMATION_WITH_SPECIFIED_SOURCE ( 'ANY', '', #12085, .NOT_KNOWN. ) ;
#9650 = VECTOR ( 'NONE', #1888, 1000.000000000000000 ) ;
#9651 = VECTOR ( 'NONE', #6265, 1000.000000000000000 ) ;
#9652 = LINE ( 'NONE', #5900, #8417 ) ;
#9653 = DIRECTION ( 'NONE',  ( 1.000000000000000000, 0.000000000000000000, 0.000000000000000000 ) ) ;
#9654 = CARTESIAN_POINT ( 'NONE',  ( 4.999999999999999112, 16.90755573046746107, -0.4834863907626340551 ) ) ;
#9655 = DIRECTION ( 'NONE',  ( -0.000000000000000000, 1.000000000000000000, -0.000000000000000000 ) ) ;
#9656 = AXIS2_PLACEMENT_3D ( 'NONE', #4131, #6018, #7198 ) ;
#9657 = ORIENTED_EDGE ( 'NONE', *, *, #980, .T. ) ;
#9658 = DIRECTION ( 'NONE',  ( 1.000000000000000000, 0.000000000000000000, 0.000000000000000000 ) ) ;
#9659 = AXIS2_PLACEMENT_3D ( 'NONE', #5117, #2998, #1123 ) ;
#9660 = DIRECTION ( 'NONE',  ( 0.000000000000000000, 0.000000000000000000, -1.000000000000000000 ) ) ;
#9661 = ORIENTED_EDGE ( 'NONE', *, *, #1719, .F. ) ;
#9662 = CARTESIAN_POINT ( 'NONE',  ( 37.00000000000000711, -2.534184013771451305, 4.310210132272582761 ) ) ;
#9663 = UNCERTAINTY_MEASURE_WITH_UNIT (LENGTH_MEASURE( 1.000000000000000082E-05 ), #10122, 'distance_accuracy_value', 'NONE');
#9664 = ORIENTED_EDGE ( 'NONE', *, *, #2273, .T. ) ;
#9665 = EDGE_CURVE ( 'NONE', #5671, #3057, #11012, .T. ) ;
#9666 = AXIS2_PLACEMENT_3D ( 'NONE', #10288, #848, #5596 ) ;
#9667 = DIRECTION ( 'NONE',  ( 1.000000000000000000, -0.000000000000000000, -0.000000000000000000 ) ) ;
#9668 = CARTESIAN_POINT ( 'NONE',  ( 0.000000000000000000, 0.000000000000000000, 0.000000000000000000 ) ) ;
#9669 = CYLINDRICAL_SURFACE ( 'NONE', #6436, 7.200000000007202416 ) ;
#9670 = DIRECTION ( 'NONE',  ( 0.000000000000000000, 0.000000000000000000, 1.000000000000000000 ) ) ;
#9671 = ORIENTED_EDGE ( 'NONE', *, *, #1950, .T. ) ;
#9672 = ORIENTED_EDGE ( 'NONE', *, *, #6277, .T. ) ;
#9673 = SHAPE_REPRESENTATION_RELATIONSHIP ( 'NONE' , 'NONE' ,  #7217, #10918 ) ;
#9674 = ORIENTED_EDGE ( 'NONE', *, *, #11112, .F. ) ;
#9675 = CARTESIAN_POINT ( 'NONE',  ( 0.000000000000000000, 0.000000000000000000, 5.000000000000000000 ) ) ;
#9676 = ITEM_DEFINED_TRANSFORMATION ( 'NONE', 'NONE', #2446,  #6056 ) ;
#9677 = CIRCLE ( 'NONE', #3285, 2.149999999999999023 ) ;
#9678 = ORIENTED_EDGE ( 'NONE', *, *, #9060, .F. ) ;
#9679 = EDGE_CURVE ( 'NONE', #7733, #9337, #12003, .T. ) ;
#9680 = EDGE_CURVE ( 'NONE', #8121, #7419, #3962, .T. ) ;
#9681 = ORIENTED_EDGE ( 'NONE', *, *, #2140, .F. ) ;
#9682 = ADVANCED_FACE ( 'NONE', ( #9909, #7098 ), #9961, .T. ) ;
#9683 = VERTEX_POINT ( 'NONE', #4325 ) ;
#9684 = DIRECTION ( 'NONE',  ( 0.000000000000000000, 0.000000000000000000, -1.000000000000000000 ) ) ;
#9685 = CIRCLE ( 'NONE', #4277, 2.500000000000000444 ) ;
#9686 = CARTESIAN_POINT ( 'NONE',  ( 4.999999999999999112, 5.622796541391564595, 13.09267581720868989 ) ) ;
#9687 = CYLINDRICAL_SURFACE ( 'NONE', #815, 9.600000000009600853 ) ;
#9688 = EDGE_LOOP ( 'NONE', ( #4931, #3159, #6138, #6148 ) ) ;
#9689 = CARTESIAN_POINT ( 'NONE',  ( 51.00000000000000000, -3.499999999999998668, -38.49999999999998579 ) ) ;
#9690 = VERTEX_POINT ( 'NONE', #10031 ) ;
#9691 = ORIENTED_EDGE ( 'NONE', *, *, #3192, .F. ) ;
#9692 = FACE_OUTER_BOUND ( 'NONE', #10210, .T. ) ;
#9693 = AXIS2_PLACEMENT_3D ( 'NONE', #3890, #8642, #1002 ) ;
#9694 = EDGE_LOOP ( 'NONE', ( #1472, #7511, #6940, #9672 ) ) ;
#9695 = CARTESIAN_POINT ( 'NONE',  ( 0.000000000000000000, 0.000000000000000000, -1.000000000000000000 ) ) ;
#9696 = EDGE_CURVE ( 'NONE', #12289, #8910, #9446, .T. ) ;
#9697 = ADVANCED_FACE ( 'NONE', ( #5143 ), #10773, .T. ) ;
#9698 = EDGE_CURVE ( 'NONE', #11007, #8473, #9154, .T. ) ;
#9699 = CARTESIAN_POINT ( 'NONE',  ( 1.400000000000001910, 6.184466335694134054E-16, 5.000000000000000000 ) ) ;
#9700 = ORIENTED_EDGE ( 'NONE', *, *, #658, .T. ) ;
#9701 = CIRCLE ( 'NONE', #2909, 20.24900000002024925 ) ;
#9702 = DIRECTION ( 'NONE',  ( -1.000000000000000000, 0.000000000000000000, 0.000000000000000000 ) ) ;
#9703 = DIRECTION ( 'NONE',  ( 0.000000000000000000, 0.000000000000000000, 1.000000000000000000 ) ) ;
#9704 = ORIENTED_EDGE ( 'NONE', *, *, #2090, .T. ) ;
#9705 = SURFACE_STYLE_USAGE ( .BOTH. , #8756 ) ;
#9706 = DIRECTION ( 'NONE',  ( 1.000000000000000000, 0.000000000000000000, 0.000000000000000000 ) ) ;
#9707 = LINE ( 'NONE', #7828, #11867 ) ;
#9708 = ADVANCED_FACE ( 'NONE', ( #8154 ), #5204, .F. ) ;
#9709 = SHAPE_REPRESENTATION ( 'MAS-168', ( #652, #4648, #5442, #11434, #8855, #4841, #6053, #8053, #3857, #4050, #12021, #10044, #2446, #11629, #61, #6250, #9445, #5244, #11031 ), #49 ) ;
#9710 = VERTEX_POINT ( 'NONE', #2276 ) ;
#9711 = CARTESIAN_POINT ( 'NONE',  ( 45.00000000000001421, 46.00000000000001421, -41.99999999999999289 ) ) ;
#9712 = EDGE_CURVE ( 'NONE', #3605, #9928, #8247, .T. ) ;
#9713 = DIRECTION ( 'NONE',  ( -1.000000000000000000, -0.000000000000000000, -0.000000000000000000 ) ) ;
#9714 = CARTESIAN_POINT ( 'NONE',  ( 4.999999999999999112, -19.24938187143300539, 6.283573709965241783 ) ) ;
#9715 = FACE_OUTER_BOUND ( 'NONE', #8350, .T. ) ;
#9716 = DIRECTION ( 'NONE',  ( -1.000000000000000000, 0.000000000000000000, 0.000000000000000000 ) ) ;
#9717 = ORIENTED_EDGE ( 'NONE', *, *, #7974, .F. ) ;
#9718 = CARTESIAN_POINT ( 'NONE',  ( 1.600000000000000089, 3.306546357697853733E-16, -2.700000000000000178 ) ) ;
#9719 = DIRECTION ( 'NONE',  ( 1.000000000000000000, 0.000000000000000000, 0.000000000000000000 ) ) ;
#9720 = ORIENTED_EDGE ( 'NONE', *, *, #3959, .F. ) ;
#9721 = DIRECTION ( 'NONE',  ( 0.000000000000000000, 0.000000000000000000, -1.000000000000000000 ) ) ;
#9722 = EDGE_CURVE ( 'NONE', #6501, #2328, #11820, .T. ) ;
#9723 = ORIENTED_EDGE ( 'NONE', *, *, #7139, .F. ) ;
#9724 = DIRECTION ( 'NONE',  ( -1.000000000000000000, 0.000000000000000000, 0.000000000000000000 ) ) ;
#9725 = CARTESIAN_POINT ( 'NONE',  ( 51.00000000000000711, 46.00000000000001421, -38.00000000000000000 ) ) ;
#9726 = LINE ( 'NONE', #458, #5754 ) ;
#9727 = DIRECTION ( 'NONE',  ( -1.000000000000000000, 0.000000000000000000, 0.000000000000000000 ) ) ;
#9728 = DIRECTION ( 'NONE',  ( 0.000000000000000000, 0.000000000000000000, 1.000000000000000000 ) ) ;
#9729 = ORIENTED_EDGE ( 'NONE', *, *, #9866, .F. ) ;
#9730 = CARTESIAN_POINT ( 'NONE',  ( 20.00000000000000000, 3.061616997868383043E-15, 25.00000000000000000 ) ) ;
#9731 = ORIENTED_EDGE ( 'NONE', *, *, #3142, .F. ) ;
#9732 = EDGE_CURVE ( 'NONE', #8609, #2734, #2325, .T. ) ;
#9733 = LINE ( 'NONE', #1976, #7284 ) ;
#9734 = ITEM_DEFINED_TRANSFORMATION ( 'NONE', 'NONE', #5442,  #6056 ) ;
#9735 = ORIENTED_EDGE ( 'NONE', *, *, #5306, .F. ) ;
#9736 = ORIENTED_EDGE ( 'NONE', *, *, #9722, .T. ) ;
#9737 = ORIENTED_EDGE ( 'NONE', *, *, #8147, .F. ) ;
#9738 = CARTESIAN_POINT ( 'NONE',  ( 20.00000000000000000, 44.00000000000002132, -12.50000000000000000 ) ) ;
#9739 = LINE ( 'NONE', #8611, #1218 ) ;
#9740 = CYLINDRICAL_SURFACE ( 'NONE', #10402, 5.000000000000000000 ) ;
#9741 = CARTESIAN_POINT ( 'NONE',  ( 26.00000000000000355, 0.000000000000000000, -48.00000000000000000 ) ) ;
#9742 = EDGE_CURVE ( 'NONE', #11003, #8470, #4271, .T. ) ;
#9743 = ORIENTED_EDGE ( 'NONE', *, *, #4474, .T. ) ;
#9744 = ORIENTED_EDGE ( 'NONE', *, *, #2284, .F. ) ;
#9745 = EDGE_CURVE ( 'NONE', #1101, #1358, #642, .T. ) ;
#9746 = ORIENTED_EDGE ( 'NONE', *, *, #10305, .F. ) ;
#9747 = DIRECTION ( 'NONE',  ( -1.000000000000000000, 0.000000000000000000, 0.000000000000000000 ) ) ;
#9748 = VERTEX_POINT ( 'NONE', #11019 ) ;
#9749 = PLANE ( 'NONE',  #3964 ) ;
#9750 = DIRECTION ( 'NONE',  ( -1.000000000000000000, 0.000000000000000000, -0.000000000000000000 ) ) ;
#9751 = EDGE_CURVE ( 'NONE', #10090, #10717, #7652, .T. ) ;
#9752 = ORIENTED_EDGE ( 'NONE', *, *, #9584, .T. ) ;
#9753 = FACE_OUTER_BOUND ( 'NONE', #9874, .T. ) ;
#9754 = DIRECTION ( 'NONE',  ( 1.000000000000000000, 0.000000000000000000, 0.000000000000000000 ) ) ;
#9755 = ORIENTED_EDGE ( 'NONE', *, *, #7709, .F. ) ;
#9756 = DIRECTION ( 'NONE',  ( 0.000000000000000000, -1.000000000000000000, 0.000000000000000000 ) ) ;
#9757 = ADVANCED_FACE ( 'NONE', ( #8967 ), #388, .T. ) ;
#9758 =( NAMED_UNIT ( * ) PLANE_ANGLE_UNIT ( ) SI_UNIT ( $, .RADIAN. ) );
#9759 = CYLINDRICAL_SURFACE ( 'NONE', #6653, 5.000000000000000000 ) ;
#9760 = ADVANCED_FACE ( 'NONE', ( #8043 ), #10947, .T. ) ;
#9761 = EDGE_CURVE ( 'NONE', #11750, #8156, #11032, .T. ) ;
#9762 = CARTESIAN_POINT ( 'NONE',  ( 1.095413108702814053, 0.000000000000000000, -3.885863436426969297 ) ) ;
#9763 = VERTEX_POINT ( 'NONE', #6282 ) ;
#9764 = CARTESIAN_POINT ( 'NONE',  ( 36.00000000000000000, 30.00000000000000711, 20.00000000000001066 ) ) ;
#9765 = CIRCLE ( 'NONE', #6156, 40.00000000000000711 ) ;
#9766 = TOROIDAL_SURFACE ( 'NONE', #4570, 5.100000000000000533, 0.1000000000000001582 ) ;
#9767 = FILL_AREA_STYLE ('',( #1188 ) ) ;
#9768 = CARTESIAN_POINT ( 'NONE',  ( 26.00000000000000355, 30.00000000000000711, 20.00000000000001066 ) ) ;
#9769 = CARTESIAN_POINT ( 'NONE',  ( 4.999999999999999112, -21.74405275335753984, -5.984728032765188388 ) ) ;
#9770 = DIRECTION ( 'NONE',  ( -1.000000000000000000, 0.000000000000000000, 0.000000000000000000 ) ) ;
#9771 = VERTEX_POINT ( 'NONE', #1521 ) ;
#9772 = CARTESIAN_POINT ( 'NONE',  ( 4.999999999999999112, 8.872489362018189496, 14.40062958310468666 ) ) ;
#9773 = CARTESIAN_POINT ( 'NONE',  ( 4.999999999999999112, -22.37914155802283034, 6.808078995945121115 ) ) ;
#9774 = PRODUCT_DEFINITION ( 'UNKNOWN', '', #1643, #2377 ) ;
#9775 = AXIS2_PLACEMENT_3D ( 'NONE', #8070, #11967, #10978 ) ;
#9776 = ORIENTED_EDGE ( 'NONE', *, *, #3296, .T. ) ;
#9777 = DIRECTION ( 'NONE',  ( -1.000000000000000000, 0.000000000000000000, -0.000000000000000000 ) ) ;
#9778 = VECTOR ( 'NONE', #8129, 1000.000000000000000 ) ;
#9779 = VERTEX_POINT ( 'NONE', #1277 ) ;
#9780 = CARTESIAN_POINT ( 'NONE',  ( 4.999999999999999112, 17.79862902732265084, 13.85025647830063100 ) ) ;
#9781 = CIRCLE ( 'NONE', #1376, 20.24900000002024569 ) ;
#9782 = DIRECTION ( 'NONE',  ( -1.000000000000000000, -0.000000000000000000, -0.000000000000000000 ) ) ;
#9783 = CIRCLE ( 'NONE', #4980, 14.24900000001425049 ) ;
#9784 = ADVANCED_FACE ( 'NONE', ( #5089 ), #328, .T. ) ;
#9785 = B_SPLINE_CURVE_WITH_KNOTS ( 'NONE', 3,
 ( #6754, #5814, #5743, #9565, #1940, #5888, #995, #4810 ),
 .UNSPECIFIED., .F., .F.,
 ( 4, 2, 2, 4 ),
 ( 0.001169467769275536707, 0.002016047890428424548, 0.002439337951004867493, 0.002862628011581310871 ),
 .UNSPECIFIED. ) ;
#9786 = EDGE_CURVE ( 'NONE', #3803, #6352, #1646, .T. ) ;
#9787 = AXIS2_PLACEMENT_3D ( 'NONE', #5043, #337, #4102 ) ;
#9788 = DIRECTION ( 'NONE',  ( -1.000000000000000000, -0.000000000000000000, -0.000000000000000000 ) ) ;
#9789 = CYLINDRICAL_SURFACE ( 'NONE', #6230, 7.500000000000000888 ) ;
#9790 = ORIENTED_EDGE ( 'NONE', *, *, #9403, .T. ) ;
#9791 = DIRECTION ( 'NONE',  ( 0.000000000000000000, 0.4999999999999950040, 0.8660254037844414832 ) ) ;
#9792 = ORIENTED_EDGE ( 'NONE', *, *, #946, .T. ) ;
#9793 = LINE ( 'NONE', #5148, #2885 ) ;
#9794 = ITEM_DEFINED_TRANSFORMATION ( 'NONE', 'NONE', #4648,  #6056 ) ;
#9795 = VERTEX_POINT ( 'NONE', #10203 ) ;
#9796 = MECHANICAL_DESIGN_GEOMETRIC_PRESENTATION_REPRESENTATION (  '', ( #1993 ), #7194 ) ;
#9797 = CARTESIAN_POINT ( 'NONE',  ( 4.999999999999999112, 8.527191590521072229, 11.41582255376076027 ) ) ;
#9798 = ORIENTED_EDGE ( 'NONE', *, *, #5463, .T. ) ;
#9799 = DIRECTION ( 'NONE',  ( 0.1305261922200524616, -0.9914448613738103822, 0.000000000000000000 ) ) ;
#9800 = CARTESIAN_POINT ( 'NONE',  ( 0.000000000000000000, 0.5999999999999998668, -2.622672778259560467 ) ) ;
#9801 = DIRECTION ( 'NONE',  ( 0.000000000000000000, 0.6828850436591804574, 0.7305258497456468270 ) ) ;
#9802 = CARTESIAN_POINT ( 'NONE',  ( -33.00000000000000000, 0.000000000000000000, -7.500000000000000888 ) ) ;
#9803 = VERTEX_POINT ( 'NONE', #5518 ) ;
#9804 = VECTOR ( 'NONE', #7197, 1000.000000000000000 ) ;
#9805 = CIRCLE ( 'NONE', #8203, 6.750000000000000000 ) ;
#9806 = VERTEX_POINT ( 'NONE', #3522 ) ;
#9807 = ORIENTED_EDGE ( 'NONE', *, *, #10981, .T. ) ;
#9808 = CARTESIAN_POINT ( 'NONE',  ( 4.999999999999999112, -1.561154383803364798, 20.18872947935930640 ) ) ;
#9809 = ORIENTED_EDGE ( 'NONE', *, *, #2493, .F. ) ;
#9810 = DIRECTION ( 'NONE',  ( 0.000000000000000000, -6.982962677686267499E-15, 1.000000000000000000 ) ) ;
#9811 = AXIS2_PLACEMENT_3D ( 'NONE', #8519, #1827, #11445 ) ;
#9812 = TOROIDAL_SURFACE ( 'NONE', #10188, 2.700000000000000622, 0.2000000000000000111 ) ;
#9813 = VECTOR ( 'NONE', #10539, 1000.000000000000000 ) ;
#9814 = CARTESIAN_POINT ( 'NONE',  ( 50.00005079999999680, 6.799999999999999822, -1.500000000000000000 ) ) ;
#9815 = ADVANCED_FACE ( 'NONE', ( #9338 ), #8281, .T. ) ;
#9816 = ORIENTED_EDGE ( 'NONE', *, *, #11274, .T. ) ;
#9818 = DIRECTION ( 'NONE',  ( -1.000000000000000000, -0.000000000000000000, -0.000000000000000000 ) ) ;
#9817 = AXIS2_PLACEMENT_3D ( 'NONE', #3040, #4780, #5721 ) ;
#9819 = DIRECTION ( 'NONE',  ( 0.000000000000000000, 0.000000000000000000, -1.000000000000000000 ) ) ;
#9820 = VECTOR ( 'NONE', #7687, 1000.000000000000000 ) ;
#9821 = ORIENTED_EDGE ( 'NONE', *, *, #3043, .T. ) ;
#9822 = VECTOR ( 'NONE', #9048, 1000.000000000000000 ) ;
#9823 = CIRCLE ( 'NONE', #8019, 25.00000000000000000 ) ;
#9824 = DIRECTION ( 'NONE',  ( 0.000000000000000000, 0.000000000000000000, 1.000000000000000000 ) ) ;
#9825 = CIRCLE ( 'NONE', #30, 9.600000000009600853 ) ;
#9826 = DIRECTION ( 'NONE',  ( 0.000000000000000000, 0.000000000000000000, -1.000000000000000000 ) ) ;
#9827 = ORIENTED_EDGE ( 'NONE', *, *, #4335, .F. ) ;
#9828 = DIRECTION ( 'NONE',  ( 0.000000000000000000, 0.000000000000000000, -1.000000000000000000 ) ) ;
#9829 = EDGE_CURVE ( 'NONE', #9537, #2623, #4516, .T. ) ;
#9830 = COLOUR_RGB ( '',1.000000000000000000, 0.9490196078431372140, 0.9098039215686274384 ) ;
#9831 = VECTOR ( 'NONE', #842, 1000.000000000000000 ) ;
#9832 = AXIS2_PLACEMENT_3D ( 'NONE', #7958, #4371, #3379 ) ;
#9833 = PRODUCT_DEFINITION_SHAPE ( 'NONE', 'NONE',  #12360 ) ;
#9834 = DIRECTION ( 'NONE',  ( -1.000000000000000000, 0.000000000000000000, 0.000000000000000000 ) ) ;
#9835 = EDGE_CURVE ( 'NONE', #6433, #10549, #5647, .T. ) ;
#9836 = CIRCLE ( 'NONE', #6837, 9.600000000009599077 ) ;
#9837 = CIRCLE ( 'NONE', #4431, 2.396904916527699214 ) ;
#9838 = EDGE_CURVE ( 'NONE', #4672, #4082, #9248, .T. ) ;
#9839 = CARTESIAN_POINT ( 'NONE',  ( 1.500000000000001332, 0.000000000000000000, 0.000000000000000000 ) ) ;
#9840 = CARTESIAN_POINT ( 'NONE',  ( 4.999999999999999112, 21.74405275335758247, 15.58472803277463825 ) ) ;
#9841 = DIRECTION ( 'NONE',  ( -1.000000000000000000, 0.000000000000000000, -0.000000000000000000 ) ) ;
#9842 = ORIENTED_EDGE ( 'NONE', *, *, #9454, .F. ) ;
#9843 = DIRECTION ( 'NONE',  ( 0.000000000000000000, 0.000000000000000000, 1.000000000000000000 ) ) ;
#9844 = DIRECTION ( 'NONE',  ( 0.000000000000000000, 0.000000000000000000, 1.000000000000000000 ) ) ;
#9845 = COLOUR_RGB ( '',1.000000000000000000, 0.9490196078431372140, 0.9098039215686274384 ) ;
#9846 = AXIS2_PLACEMENT_3D ( 'NONE', #7218, #4089, #2209 ) ;
#9847 = ORIENTED_EDGE ( 'NONE', *, *, #1397, .T. ) ;
#9848 = CARTESIAN_POINT ( 'NONE',  ( 5.686050877451574337, -5.768780236673276995, -1.000000000000000000 ) ) ;
#9849 = CIRCLE ( 'NONE', #7439, 5.000000000000000000 ) ;
#9850 = VECTOR ( 'NONE', #10032, 1000.000000000000000 ) ;
#9851 = ORIENTED_EDGE ( 'NONE', *, *, #12024, .T. ) ;
#9852 = DIRECTION ( 'NONE',  ( 0.000000000000000000, 0.000000000000000000, -1.000000000000000000 ) ) ;
#9853 = EDGE_CURVE ( 'NONE', #4492, #7733, #6652, .T. ) ;
#9854 = DIRECTION ( 'NONE',  ( 0.000000000000000000, 0.000000000000000000, -1.000000000000000000 ) ) ;
#9855 = CIRCLE ( 'NONE', #457, 5.000000000000000000 ) ;
#9856 = EDGE_CURVE ( 'NONE', #4719, #6551, #11630, .T. ) ;
#9857 = SURFACE_SIDE_STYLE ('',( #384 ) ) ;
#9858 = CARTESIAN_POINT ( 'NONE',  ( 26.00000000000000355, 0.000000000000000000, -34.49999999999999289 ) ) ;
#9859 = VECTOR ( 'NONE', #8091, 1000.000000000000000 ) ;
#9860 = CARTESIAN_POINT ( 'NONE',  ( 2.499999999999999556, 4.576198416197250651, 26.60936692326691855 ) ) ;
#9861 = FACE_OUTER_BOUND ( 'NONE', #2576, .T. ) ;
#9862 = VERTEX_POINT ( 'NONE', #12255 ) ;
#9863 = EDGE_LOOP ( 'NONE', ( #5591, #3588, #4466, #4443 ) ) ;
#9864 = CARTESIAN_POINT ( 'NONE',  ( 0.000000000000000000, 6.283573709965571297, -19.24938187143289881 ) ) ;
#9865 = ORIENTED_EDGE ( 'NONE', *, *, #1205, .F. ) ;
#9866 = EDGE_CURVE ( 'NONE', #6238, #8693, #5848, .T. ) ;
#9867 = AXIS2_PLACEMENT_3D ( 'NONE', #9025, #446, #11875 ) ;
#9868 = EDGE_CURVE ( 'NONE', #3875, #6501, #9053, .T. ) ;
#9869 = CARTESIAN_POINT ( 'NONE',  ( 0.000000000000000000, 22.37914155802285876, -2.791921004064323864 ) ) ;
#9870 = CARTESIAN_POINT ( 'NONE',  ( 4.999999999999999112, -21.74405275335753984, -5.984728032765188388 ) ) ;
#9871 = DIRECTION ( 'NONE',  ( 1.000000000000000000, 0.000000000000000000, 0.000000000000000000 ) ) ;
#9872 = DIRECTION ( 'NONE',  ( -1.000000000000000000, -0.000000000000000000, 0.000000000000000000 ) ) ;
#9873 = DIRECTION ( 'NONE',  ( 1.000000000000000000, 0.000000000000000000, 0.000000000000000000 ) ) ;
#9874 = EDGE_LOOP ( 'NONE', ( #2543, #40, #5497, #3652 ) ) ;
#9875 = VERTEX_POINT ( 'NONE', #3581 ) ;
#9876 = VERTEX_POINT ( 'NONE', #7467 ) ;
#9877 = DIRECTION ( 'NONE',  ( 1.000000000000000000, 0.000000000000000000, 0.000000000000000000 ) ) ;
#9878 = CYLINDRICAL_SURFACE ( 'NONE', #5165, 20.24900000002024569 ) ;
#9879 = AXIS2_PLACEMENT_3D ( 'NONE', #2332, #6041, #5972 ) ;
#9880 = DIRECTION ( 'NONE',  ( 0.000000000000000000, 0.000000000000000000, -1.000000000000000000 ) ) ;
#9881 = ORIENTED_EDGE ( 'NONE', *, *, #10876, .T. ) ;
#9882 = DIRECTION ( 'NONE',  ( 0.000000000000000000, -6.982962677686266711E-15, 1.000000000000000000 ) ) ;
#9883 = CARTESIAN_POINT ( 'NONE',  ( 4.999999999999999112, 1.561154383803505796, -20.18872947935929574 ) ) ;
#9884 = EDGE_LOOP ( 'NONE', ( #5440, #3471, #1114, #7746 ) ) ;
#9885 = DIRECTION ( 'NONE',  ( 1.000000000000000000, 0.000000000000000000, -0.000000000000000000 ) ) ;
#9886 = DIRECTION ( 'NONE',  ( 0.000000000000000000, 0.000000000000000000, -1.000000000000000000 ) ) ;
#9887 = DIRECTION ( 'NONE',  ( 1.000000000000000000, 0.000000000000000000, 0.000000000000000000 ) ) ;
#9888 = ORIENTED_EDGE ( 'NONE', *, *, #3336, .F. ) ;
#9889 = CARTESIAN_POINT ( 'NONE',  ( -36.00000000000000711, 0.000000000000000000, 0.000000000000000000 ) ) ;
#9890 = CARTESIAN_POINT ( 'NONE',  ( 1.000000000000000000, 0.5999999999999998668, -4.000000000000000000 ) ) ;
#9891 = CIRCLE ( 'NONE', #12263, 5.750000000000000000 ) ;
#9892 = DIRECTION ( 'NONE',  ( 1.000000000000000000, -0.000000000000000000, -0.000000000000000000 ) ) ;
#9893 = DIRECTION ( 'NONE',  ( 0.000000000000000000, -1.000000000000000000, 0.000000000000000000 ) ) ;
#9894 = FACE_OUTER_BOUND ( 'NONE', #8986, .T. ) ;
#9895 = VERTEX_POINT ( 'NONE', #570 ) ;
#9896 = VERTEX_POINT ( 'NONE', #6337 ) ;
#9897 = ADVANCED_FACE ( 'NONE', ( #12010, #7400, #3465 ), #7287, .F. ) ;
#9898 = CARTESIAN_POINT ( 'NONE',  ( 0.000000000000000000, 15.22291137398942418, -14.46592441914948779 ) ) ;
#9899 = CARTESIAN_POINT ( 'NONE',  ( 0.000000000000000000, -13.17168466712939257, 15.37949036966207039 ) ) ;
#9900 = ORIENTED_EDGE ( 'NONE', *, *, #9454, .T. ) ;
#9901 = DIRECTION ( 'NONE',  ( 0.000000000000000000, 0.000000000000000000, -1.000000000000000000 ) ) ;
#9902 = PRODUCT_DEFINITION_CONTEXT ( 'detailed design', #2570, 'design' ) ;
#9903 = EDGE_CURVE ( 'NONE', #8693, #6875, #3650, .T. ) ;
#9904 = CONICAL_SURFACE ( 'NONE', #4700, 3.790027207537782772, 0.08726646259971644615 ) ;
#9905 = EDGE_LOOP ( 'NONE', ( #3513, #7515, #2736, #123 ) ) ;
#9906 = CARTESIAN_POINT ( 'NONE',  ( 0.000000000000000000, -5.955107813822691831, 26.33508479058318485 ) ) ;
#9907 = DIRECTION ( 'NONE',  ( 0.000000000000000000, 0.000000000000000000, 1.000000000000000000 ) ) ;
#9908 = CARTESIAN_POINT ( 'NONE',  ( 2.499999999999999556, -5.955107813822691831, 26.33508479058318485 ) ) ;
#9909 = FACE_OUTER_BOUND ( 'NONE', #3856, .T. ) ;
#9910 = DIRECTION ( 'NONE',  ( -1.000000000000000000, 0.000000000000000000, -0.000000000000000000 ) ) ;
#9911 = VERTEX_POINT ( 'NONE', #5396 ) ;
#9912 = ADVANCED_FACE ( 'NONE', ( #12070 ), #5465, .T. ) ;
#9913 = LINE ( 'NONE', #11026, #11753 ) ;
#9914 = ORIENTED_EDGE ( 'NONE', *, *, #2100, .T. ) ;
#9915 = SURFACE_SIDE_STYLE ('',( #466 ) ) ;
#9916 = EDGE_CURVE ( 'NONE', #5423, #5429, #3252, .T. ) ;
#9917 = EDGE_CURVE ( 'NONE', #2913, #2151, #8645, .T. ) ;
#9918 = ORIENTED_EDGE ( 'NONE', *, *, #9665, .F. ) ;
#9919 = EDGE_CURVE ( 'NONE', #279, #3487, #4649, .T. ) ;
#9920 = CARTESIAN_POINT ( 'NONE',  ( 51.00000000000000711, 50.00000000000000711, -38.00000000000000000 ) ) ;
#9921 = CARTESIAN_POINT ( 'NONE',  ( 4.999999999999999112, -0.4834863907624570856, -16.90755573046746463 ) ) ;
#9922 = CARTESIAN_POINT ( 'NONE',  ( 51.00000000000000000, -3.499999999999998668, -38.49999999999998579 ) ) ;
#9923 = DIRECTION ( 'NONE',  ( -1.000000000000000000, -0.000000000000000000, -0.000000000000000000 ) ) ;
#9924 = CARTESIAN_POINT ( 'NONE',  ( 27.38165010660258503, -0.8169585525225422362, -40.74199414808185793 ) ) ;
#9925 = ORIENTED_EDGE ( 'NONE', *, *, #2628, .T. ) ;
#9926 = EDGE_CURVE ( 'NONE', #11679, #6664, #5443, .T. ) ;
#9927 = CARTESIAN_POINT ( 'NONE',  ( 4.999999999999999112, 21.74405275335758247, 15.58472803277463825 ) ) ;
#9928 = VERTEX_POINT ( 'NONE', #9520 ) ;
#9929 = CARTESIAN_POINT ( 'NONE',  ( 0.000000000000000000, 0.000000000000000000, 0.000000000000000000 ) ) ;
#9930 = ORIENTED_EDGE ( 'NONE', *, *, #10243, .T. ) ;
#9931 = CARTESIAN_POINT ( 'NONE',  ( 4.999999999999999112, 6.283573709965309284, 19.24938187143298052 ) ) ;
#9932 = PRODUCT ( 'hub', 'hub', '', ( #3970 ) ) ;
#9933 = DIRECTION ( 'NONE',  ( 0.000000000000000000, 0.000000000000000000, 1.000000000000000000 ) ) ;
#9934 = CARTESIAN_POINT ( 'NONE',  ( 37.00000000000000711, -2.172883482918394282, 4.280020720704565740 ) ) ;
#9935 = EDGE_LOOP ( 'NONE', ( #6721, #7989, #8148, #4420 ) ) ;
#9936 = EDGE_CURVE ( 'NONE', #1155, #2267, #7580, .T. ) ;
#9937 = CARTESIAN_POINT ( 'NONE',  ( 2.500000000000000000, 1.178949249685213863, -2.042000000000001148 ) ) ;
#9938 = ORIENTED_EDGE ( 'NONE', *, *, #3411, .F. ) ;
#9939 = CARTESIAN_POINT ( 'NONE',  ( 36.00000000000000711, -2.172883482918394282, 4.280020720704565740 ) ) ;
#9940 = CARTESIAN_POINT ( 'NONE',  ( 15.00000000000000355, 40.00000000000000711, 0.000000000000000000 ) ) ;
#9941 = ORIENTED_EDGE ( 'NONE', *, *, #11922, .T. ) ;
#9942 = DIRECTION ( 'NONE',  ( -1.000000000000000000, -0.000000000000000000, -0.000000000000000000 ) ) ;
#9943 = DIRECTION ( 'NONE',  ( 0.000000000000000000, 0.000000000000000000, -1.000000000000000000 ) ) ;
#9944 = CARTESIAN_POINT ( 'NONE',  ( 42.00000000000000000, 1.456773409934505593E-31, -41.99999999999998579 ) ) ;
#9945 = CARTESIAN_POINT ( 'NONE',  ( -1.250000000000000000, -6.429618962271402616, 0.000000000000000000 ) ) ;
#9946 = FACE_OUTER_BOUND ( 'NONE', #2553, .T. ) ;
#9947 = DIRECTION ( 'NONE',  ( 0.000000000000000000, 0.9238795325112851842, 0.3826834323650938896 ) ) ;
#9948 = ORIENTED_EDGE ( 'NONE', *, *, #38, .T. ) ;
#9949 = ORIENTED_EDGE ( 'NONE', *, *, #2334, .T. ) ;
#9950 = CARTESIAN_POINT ( 'NONE',  ( 0.000000000000000000, 0.000000000000000000, 0.000000000000000000 ) ) ;
#9951 = LINE ( 'NONE', #557, #2633 ) ;
#9952 = ORIENTED_EDGE ( 'NONE', *, *, #2315, .F. ) ;
#9953 = DIRECTION ( 'NONE',  ( -1.000000000000000000, 0.000000000000000000, 0.000000000000000000 ) ) ;
#9954 = ORIENTED_EDGE ( 'NONE', *, *, #7367, .T. ) ;
#9955 = CARTESIAN_POINT ( 'NONE',  ( 0.000000000000000000, -0.5999999999999994227, -4.000000000000000000 ) ) ;
#9956 = CIRCLE ( 'NONE', #1764, 7.200000000007204193 ) ;
#9957 = EDGE_CURVE ( 'NONE', #9980, #5401, #51, .T. ) ;
#9958 = SURFACE_STYLE_FILL_AREA ( #2323 ) ;
#9959 = FACE_OUTER_BOUND ( 'NONE', #8238, .T. ) ;
#9960 = EDGE_CURVE ( 'NONE', #11122, #5671, #1055, .T. ) ;
#9961 = PLANE ( 'NONE',  #7046 ) ;
#9962 = DIRECTION ( 'NONE',  ( 0.000000000000000000, 0.000000000000000000, 1.000000000000000000 ) ) ;
#9963 = AXIS2_PLACEMENT_3D ( 'NONE', #8508, #5691, #8637 ) ;
#9964 = VERTEX_POINT ( 'NONE', #4758 ) ;
#9965 = CARTESIAN_POINT ( 'NONE',  ( 4.999999999999997335, 6.799999999999999822, -1.500000000000000000 ) ) ;
#9966 = VERTEX_POINT ( 'NONE', #7840 ) ;
#9967 = DIRECTION ( 'NONE',  ( 1.000000000000000000, -0.000000000000000000, -0.000000000000000000 ) ) ;
#9968 = ORIENTED_EDGE ( 'NONE', *, *, #2253, .T. ) ;
#9969 = VECTOR ( 'NONE', #5924, 1000.000000000000114 ) ;
#9970 = AXIS2_PLACEMENT_3D ( 'NONE', #11422, #5736, #7500 ) ;
#9971 = ADVANCED_FACE ( 'NONE', ( #11635 ), #4828, .F. ) ;
#9972 = CARTESIAN_POINT ( 'NONE',  ( 4.999999999999999112, -15.37949036966202598, -13.17168466712944408 ) ) ;
#9973 = AXIS2_PLACEMENT_3D ( 'NONE', #1337, #2218, #10724 ) ;
#9974 = CYLINDRICAL_SURFACE ( 'NONE', #1595, 9.600000000009600853 ) ;
#9975 = DIRECTION ( 'NONE',  ( -1.000000000000000000, -0.000000000000000000, -0.000000000000000000 ) ) ;
#9976 = ADVANCED_FACE ( 'NONE', ( #6902 ), #7658, .T. ) ;
#9977 = CARTESIAN_POINT ( 'NONE',  ( 43.00000000000000000, -3.058102613202345665, 3.699730856038719207 ) ) ;
#9979 = EDGE_CURVE ( 'NONE', #997, #7460, #2447, .T. ) ;
#9978 = CARTESIAN_POINT ( 'NONE',  ( -33.00000000000000000, 0.000000000000000000, 0.000000000000000000 ) ) ;
#9980 = VERTEX_POINT ( 'NONE', #1896 ) ;
#9981 = DIRECTION ( 'NONE',  ( -1.000000000000000000, -3.903127820947815962E-18, 0.000000000000000000 ) ) ;
#9982 = AXIS2_PLACEMENT_3D ( 'NONE', #7298, #11092, #5587 ) ;
#9983 = ORIENTED_EDGE ( 'NONE', *, *, #2803, .F. ) ;
#9984 = VECTOR ( 'NONE', #2250, 1000.000000000000000 ) ;
#9985 = DIRECTION ( 'NONE',  ( 0.000000000000000000, 0.000000000000000000, 1.000000000000000000 ) ) ;
#9986 = VERTEX_POINT ( 'NONE', #5834 ) ;
#9987 = AXIS2_PLACEMENT_3D ( 'NONE', #9890, #1258, #8950 ) ;
#9988 = CARTESIAN_POINT ( 'NONE',  ( 20.00000000000000000, 0.000000000000000000, 0.000000000000000000 ) ) ;
#9989 = EDGE_CURVE ( 'NONE', #542, #4490, #5757, .T. ) ;
#9990 = DIRECTION ( 'NONE',  ( -1.000000000000000000, -3.903127820947815962E-18, 0.000000000000000000 ) ) ;
#9991 = AXIS2_PLACEMENT_3D ( 'NONE', #10103, #11772, #7110 ) ;
#9992 = ORIENTED_EDGE ( 'NONE', *, *, #6224, .T. ) ;
#9993 = DIRECTION ( 'NONE',  ( 0.000000000000000000, -0.4526840589413320126, 0.8916709834801178625 ) ) ;
#9994 = PRODUCT_DEFINITION ( 'UNKNOWN', '', #1858, #6140 ) ;
#9995 = ORIENTED_EDGE ( 'NONE', *, *, #3163, .F. ) ;
#9996 = DIRECTION ( 'NONE',  ( 0.000000000000000000, 1.598721155460225103E-14, 1.000000000000000000 ) ) ;
#9997 = ORIENTED_EDGE ( 'NONE', *, *, #9530, .F. ) ;
#9998 =( NAMED_UNIT ( * ) SI_UNIT ( $, .STERADIAN. ) SOLID_ANGLE_UNIT ( ) );
#9999 = CARTESIAN_POINT ( 'NONE',  ( 37.00000000000000711, 0.8169585525225424583, -43.25800585191812075 ) ) ;
#10000 = CIRCLE ( 'NONE', #4596, 8.099999999999999645 ) ;
#10001 = FACE_OUTER_BOUND ( 'NONE', #3384, .T. ) ;
#10002 = AXIS2_PLACEMENT_3D ( 'NONE', #9839, #6951, #10702 ) ;
#10003 = ORIENTED_EDGE ( 'NONE', *, *, #8303, .T. ) ;
#10004 = CARTESIAN_POINT ( 'NONE',  ( 36.00000000000000711, 12.50000000000000000, -37.99671038392666134 ) ) ;
#10005 = VECTOR ( 'NONE', #2287, 1000.000000000000000 ) ;
#10006 = EDGE_CURVE ( 'NONE', #11240, #9064, #1859, .T. ) ;
#10007 = EDGE_CURVE ( 'NONE', #8024, #4406, #136, .T. ) ;
#10008 = CARTESIAN_POINT ( 'NONE',  ( 26.00000000000000355, 1.456773409934505593E-31, -41.99999999999998579 ) ) ;
#10009 = PRESENTATION_LAYER_ASSIGNMENT (  '', '', ( #11968 ) ) ;
#10010 = CIRCLE ( 'NONE', #5019, 27.00000000002699707 ) ;
#10011 = FACE_BOUND ( 'NONE', #741, .T. ) ;
#10012 = CIRCLE ( 'NONE', #3028, 20.24900000002024925 ) ;
#10013 = AXIS2_PLACEMENT_3D ( 'NONE', #5292, #6347, #1663 ) ;
#10014 = CARTESIAN_POINT ( 'NONE',  ( 45.00000000000000000, 0.000000000000000000, 0.000000000000000000 ) ) ;
#10015 = CARTESIAN_POINT ( 'NONE',  ( 4.999999999999999112, 0.000000000000000000, 0.000000000000000000 ) ) ;
#10016 = ORIENTED_EDGE ( 'NONE', *, *, #9957, .T. ) ;
#10017 = ORIENTED_EDGE ( 'NONE', *, *, #10534, .T. ) ;
#10018 = CARTESIAN_POINT ( 'NONE',  ( 1.000000000000000000, -0.5999999999999995337, -3.826895796574397046 ) ) ;
#10019 = DIRECTION ( 'NONE',  ( 0.000000000000000000, 0.000000000000000000, 1.000000000000000000 ) ) ;
#10020 = ORIENTED_EDGE ( 'NONE', *, *, #9960, .T. ) ;
#10021 = DIRECTION ( 'NONE',  ( 0.000000000000000000, 0.000000000000000000, -1.000000000000000000 ) ) ;
#10022 = ORIENTED_EDGE ( 'NONE', *, *, #189, .F. ) ;
#10023 = FACE_OUTER_BOUND ( 'NONE', #6040, .T. ) ;
#10024 = MECHANICAL_DESIGN_GEOMETRIC_PRESENTATION_REPRESENTATION (  '', ( #11011 ), #10618 ) ;
#10025 = AXIS2_PLACEMENT_3D ( 'NONE', #6596, #10401, #1852 ) ;
#10026 = VECTOR ( 'NONE', #10768, 1000.000000000000000 ) ;
#10027 = VERTEX_POINT ( 'NONE', #3896 ) ;
#10028 =( LENGTH_UNIT ( ) NAMED_UNIT ( * ) SI_UNIT ( .MILLI., .METRE. ) );
#10029 = FACE_OUTER_BOUND ( 'NONE', #335, .T. ) ;
#10030 =( GEOMETRIC_REPRESENTATION_CONTEXT ( 3 ) GLOBAL_UNCERTAINTY_ASSIGNED_CONTEXT ( ( #6666 ) ) GLOBAL_UNIT_ASSIGNED_CONTEXT ( ( #3804, #11241, #9370 ) ) REPRESENTATION_CONTEXT ( 'NONE', 'WORKASPACE' ) );
#10031 = CARTESIAN_POINT ( 'NONE',  ( 2.500000000000000000, -2.629050547790028551E-15, -2.041999999999999815 ) ) ;
#10032 = DIRECTION ( 'NONE',  ( -1.000000000000000000, 0.000000000000000000, 0.000000000000000000 ) ) ;
#10033 = VECTOR ( 'NONE', #6731, 1000.000000000000114 ) ;
#10034 = CIRCLE ( 'NONE', #6241, 4.799999999999999822 ) ;
#10035 = PRODUCT_DEFINITION_SHAPE ( 'NONE', 'NONE',  #12364 ) ;
#10036 = ORIENTED_EDGE ( 'NONE', *, *, #8327, .T. ) ;
#10037 = LINE ( 'NONE', #646, #7576 ) ;
#10038 = VECTOR ( 'NONE', #8582, 1000.000000000000000 ) ;
#10039 = CARTESIAN_POINT ( 'NONE',  ( -20.63749999999999929, 7.041719095097280880E-16, 5.750000000000000000 ) ) ;
#10040 = ORIENTED_EDGE ( 'NONE', *, *, #16, .F. ) ;
#10041 = DIRECTION ( 'NONE',  ( 1.000000000000000000, -0.000000000000000000, 0.000000000000000000 ) ) ;
#10042 = VERTEX_POINT ( 'NONE', #890 ) ;
#10043 = ADVANCED_FACE ( 'NONE', ( #7716 ), #10570, .T. ) ;
#10044 = AXIS2_PLACEMENT_3D ( 'NONE', #12037, #2411, #6237 ) ;
#10045 = AXIS2_PLACEMENT_3D ( 'NONE', #5, #3832, #1954 ) ;
#10046 =( GEOMETRIC_REPRESENTATION_CONTEXT ( 3 ) GLOBAL_UNCERTAINTY_ASSIGNED_CONTEXT ( ( #12262 ) ) GLOBAL_UNIT_ASSIGNED_CONTEXT ( ( #7917, #1097, #9539 ) ) REPRESENTATION_CONTEXT ( 'NONE', 'WORKASPACE' ) );
#10047 = DIRECTION ( 'NONE',  ( -1.000000000000000000, 0.000000000000000000, -0.000000000000000000 ) ) ;
#10048 = DIRECTION ( 'NONE',  ( 1.000000000000000000, 0.000000000000000000, 0.000000000000000000 ) ) ;
#10049 = DIRECTION ( 'NONE',  ( 0.000000000000000000, 0.000000000000000000, -1.000000000000000000 ) ) ;
#10050 = DIRECTION ( 'NONE',  ( 0.000000000000000000, -0.9238795325112827417, -0.3826834323650997738 ) ) ;
#10051 = VERTEX_POINT ( 'NONE', #8521 ) ;
#10052 = DIRECTION ( 'NONE',  ( -1.000000000000000000, 0.000000000000000000, 0.000000000000000000 ) ) ;
#10053 = VERTEX_POINT ( 'NONE', #4892 ) ;
#10054 = EDGE_CURVE ( 'NONE', #1657, #3871, #7056, .T. ) ;
#10055 = CARTESIAN_POINT ( 'NONE',  ( 27.49999999999999645, 0.000000000000000000, -41.99999999999999289 ) ) ;
#10056 = VECTOR ( 'NONE', #11682, 1000.000000000000000 ) ;
#10057 = ORIENTED_EDGE ( 'NONE', *, *, #7096, .T. ) ;
#10058 = CARTESIAN_POINT ( 'NONE',  ( 0.000000000000000000, 0.5999999999999998668, -2.622672778259560467 ) ) ;
#10059 = EDGE_CURVE ( 'NONE', #11181, #7180, #3759, .T. ) ;
#10060 = CARTESIAN_POINT ( 'NONE',  ( -0.5590169943749470072, 0.000000000000000000, 0.000000000000000000 ) ) ;
#10061 = EDGE_LOOP ( 'NONE', ( #10851, #3667, #6791, #9253 ) ) ;
#10062 = CARTESIAN_POINT ( 'NONE',  ( 4.999999999999999112, -8.872489362018088244, -14.40062958310474883 ) ) ;
#10063 = MECHANICAL_DESIGN_GEOMETRIC_PRESENTATION_REPRESENTATION (  '', ( #3083 ), #6072 ) ;
#10064 = ORIENTED_EDGE ( 'NONE', *, *, #60, .F. ) ;
#10065 = DIRECTION ( 'NONE',  ( 1.000000000000000000, 0.000000000000000000, 0.000000000000000000 ) ) ;
#10066 = ORIENTED_EDGE ( 'NONE', *, *, #7715, .F. ) ;
#10067 =( LENGTH_UNIT ( ) NAMED_UNIT ( * ) SI_UNIT ( .MILLI., .METRE. ) );
#10068 = CARTESIAN_POINT ( 'NONE',  ( 4.999999999999999112, 0.000000000000000000, 0.000000000000000000 ) ) ;
#10069 = EDGE_CURVE ( 'NONE', #11069, #8903, #10457, .T. ) ;
#10070 = PRESENTATION_LAYER_ASSIGNMENT (  '', '', ( #6278 ) ) ;
#10072 = VERTEX_POINT ( 'NONE', #5902 ) ;
#10071 = EDGE_CURVE ( 'NONE', #8607, #1747, #6456, .T. ) ;
#10073 = CARTESIAN_POINT ( 'NONE',  ( 37.00000000000000711, -3.606021680338235225, -38.83193945118931367 ) ) ;
#10074 = ADVANCED_FACE ( 'NONE', ( #9715 ), #4946, .T. ) ;
#10075 = CARTESIAN_POINT ( 'NONE',  ( 43.00000000000000000, -3.058102613202345665, 3.699730856038719207 ) ) ;
#10076 = CYLINDRICAL_SURFACE ( 'NONE', #6005, 27.00000000002699707 ) ;
#10077 = AXIS2_PLACEMENT_3D ( 'NONE', #9848, #1201, #11878 ) ;
#10078 = DIRECTION ( 'NONE',  ( 1.000000000000000000, 0.000000000000000000, 0.000000000000000000 ) ) ;
#10079 = DIRECTION ( 'NONE',  ( -1.000000000000000000, -0.000000000000000000, -0.000000000000000000 ) ) ;
#10080 = ORIENTED_EDGE ( 'NONE', *, *, #8853, .F. ) ;
#10081 = ORIENTED_EDGE ( 'NONE', *, *, #10876, .F. ) ;
#10082 = DIRECTION ( 'NONE',  ( 1.000000000000000000, -0.000000000000000000, -0.000000000000000000 ) ) ;
#10083 = EDGE_CURVE ( 'NONE', #11670, #6904, #11827, .T. ) ;
#10084 = DIRECTION ( 'NONE',  ( -0.000000000000000000, 0.000000000000000000, 1.000000000000000000 ) ) ;
#10085 = EDGE_LOOP ( 'NONE', ( #7529, #1469, #6460 ) ) ;
#10086 = CARTESIAN_POINT ( 'NONE',  ( 4.999999999999999112, 22.37914155802281257, 2.791921004064645384 ) ) ;
#10087 = ORIENTED_EDGE ( 'NONE', *, *, #6947, .T. ) ;
#10088 = FACE_OUTER_BOUND ( 'NONE', #770, .T. ) ;
#10089 = AXIS2_PLACEMENT_3D ( 'NONE', #1752, #3698, #2890 ) ;
#10090 = VERTEX_POINT ( 'NONE', #11813 ) ;
#10091 = LINE ( 'NONE', #6280, #6196 ) ;
#10092 = CARTESIAN_POINT ( 'NONE',  ( 2.500000000000000000, 0.000000000000000000, 0.000000000000000000 ) ) ;
#10093 = DIRECTION ( 'NONE',  ( 0.000000000000000000, 0.000000000000000000, 1.000000000000000000 ) ) ;
#10094 = DIRECTION ( 'NONE',  ( 0.000000000000000000, 0.000000000000000000, -1.000000000000000000 ) ) ;
#10095 = EDGE_LOOP ( 'NONE', ( #8550, #9930, #9096, #390 ) ) ;
#10096 = CARTESIAN_POINT ( 'NONE',  ( 33.00000000000000000, 0.000000000000000000, -41.99999999999999289 ) ) ;
#10097 = VECTOR ( 'NONE', #6257, 1000.000000000000000 ) ;
#10098 = EDGE_CURVE ( 'NONE', #9771, #11527, #5257, .T. ) ;
#10099 = DIRECTION ( 'NONE',  ( 0.000000000000000000, -1.000000000000000000, 1.471414886128461471E-15 ) ) ;
#10100 = ORIENTED_EDGE ( 'NONE', *, *, #10376, .F. ) ;
#10101 = ORIENTED_EDGE ( 'NONE', *, *, #499, .F. ) ;
#10102 = LINE ( 'NONE', #3531, #781 ) ;
#10103 = CARTESIAN_POINT ( 'NONE',  ( 0.000000000000000000, -22.37914155802287297, 2.791921004064167544 ) ) ;
#10104 = CARTESIAN_POINT ( 'NONE',  ( 45.00000000000000000, 0.000000000000000000, 0.000000000000000000 ) ) ;
#10105 = CARTESIAN_POINT ( 'NONE',  ( 0.000000000000000000, 0.000000000000000000, 0.000000000000000000 ) ) ;
#10106 = DIRECTION ( 'NONE',  ( -1.000000000000000000, -0.000000000000000000, -0.000000000000000000 ) ) ;
#10107 = ORIENTED_EDGE ( 'NONE', *, *, #7325, .T. ) ;
#10108 = CARTESIAN_POINT ( 'NONE',  ( -26.00000000000000355, -7.960204194457796463E-16, -6.500000000000000888 ) ) ;
#10109 = VERTEX_POINT ( 'NONE', #8090 ) ;
#10110 = SURFACE_STYLE_USAGE ( .BOTH. , #7357 ) ;
#10111 = DIRECTION ( 'NONE',  ( 1.000000000000000000, 0.000000000000000000, 0.000000000000000000 ) ) ;
#10112 = VERTEX_POINT ( 'NONE', #1370 ) ;
#10113 = LINE ( 'NONE', #5236, #817 ) ;
#10114 = DIRECTION ( 'NONE',  ( 1.000000000000000000, 0.000000000000000000, 0.000000000000000000 ) ) ;
#10115 = ORIENTED_EDGE ( 'NONE', *, *, #5543, .F. ) ;
#10116 = LINE ( 'NONE', #7316, #5598 ) ;
#10117 = EDGE_CURVE ( 'NONE', #5845, #11069, #1447, .T. ) ;
#10118 = EDGE_CURVE ( 'NONE', #9337, #10885, #9855, .T. ) ;
#10119 = VERTEX_POINT ( 'NONE', #7016 ) ;
#10120 = DIRECTION ( 'NONE',  ( 0.5150380737757255245, 0.000000000000000000, -0.8571673013836856869 ) ) ;
#10121 = ORIENTED_EDGE ( 'NONE', *, *, #1116, .F. ) ;
#10122 =( LENGTH_UNIT ( ) NAMED_UNIT ( * ) SI_UNIT ( .MILLI., .METRE. ) );
#10123 = PLANE ( 'NONE',  #8502 ) ;
#10124 = ORIENTED_EDGE ( 'NONE', *, *, #7379, .F. ) ;
#10125 = PLANE ( 'NONE',  #9254 ) ;
#10126 = DIRECTION ( 'NONE',  ( 0.000000000000000000, 0.7071067811865487940, -0.7071067811865462405 ) ) ;
#10127 = EDGE_CURVE ( 'NONE', #3842, #9428, #11871, .T. ) ;
#10128 = CARTESIAN_POINT ( 'NONE',  ( 15.00000000000000355, 40.00000000000000711, 0.000000000000000000 ) ) ;
#10129 = EDGE_CURVE ( 'NONE', #10139, #12254, #2652, .T. ) ;
#10130 = CARTESIAN_POINT ( 'NONE',  ( 4.999999999999999112, 21.74405275335766419, -5.984728032764733641 ) ) ;
#10131 = FACE_OUTER_BOUND ( 'NONE', #3123, .T. ) ;
#10132 = ADVANCED_FACE ( 'NONE', ( #7900 ), #3145, .T. ) ;
#10133 = VERTEX_POINT ( 'NONE', #5262 ) ;
#10134 = VERTEX_POINT ( 'NONE', #9088 ) ;
#10135 = PLANE ( 'NONE',  #861 ) ;
#10136 = CARTESIAN_POINT ( 'NONE',  ( 4.999999999999999112, 22.83261415639523051, -14.41081992069284645 ) ) ;
#10137 = EDGE_LOOP ( 'NONE', ( #10986, #3800, #1778, #578 ) ) ;
#10138 = CARTESIAN_POINT ( 'NONE',  ( 37.00000000000000711, -2.432816653220593039, 4.137801726981678030 ) ) ;
#10139 = VERTEX_POINT ( 'NONE', #6952 ) ;
#10140 = CARTESIAN_POINT ( 'NONE',  ( -15.00000000000000000, 44.00000000000001421, 0.000000000000000000 ) ) ;
#10141 = PRESENTATION_STYLE_ASSIGNMENT (( #1700 ) ) ;
#10142 = CARTESIAN_POINT ( 'NONE',  ( -25.00000000000000000, 0.000000000000000000, 25.00000000000000000 ) ) ;
#10143 = CARTESIAN_POINT ( 'NONE',  ( 4.999999999999999112, 22.37914155802285876, -2.791921004064323864 ) ) ;
#10144 = CARTESIAN_POINT ( 'NONE',  ( 45.00000000000001421, 50.00000000000000711, -38.00000000000000000 ) ) ;
#10145 = ORIENTED_EDGE ( 'NONE', *, *, #9369, .T. ) ;
#10146 = DIRECTION ( 'NONE',  ( -1.000000000000000000, -0.000000000000000000, -0.000000000000000000 ) ) ;
#10147 = CARTESIAN_POINT ( 'NONE',  ( -20.63749999999999574, 0.000000000000000000, 0.000000000000000000 ) ) ;
#10148 = VERTEX_POINT ( 'NONE', #11691 ) ;
#10149 = DIRECTION ( 'NONE',  ( 0.000000000000000000, 0.000000000000000000, 1.000000000000000000 ) ) ;
#10150 = ORIENTED_EDGE ( 'NONE', *, *, #5307, .F. ) ;
#10151 = VECTOR ( 'NONE', #2385, 1000.000000000000000 ) ;
#10152 = EDGE_CURVE ( 'NONE', #11478, #720, #10435, .T. ) ;
#10153 = CARTESIAN_POINT ( 'NONE',  ( -0.5590169943749470072, 0.000000000000000000, 0.000000000000000000 ) ) ;
#10154 = EDGE_CURVE ( 'NONE', #12088, #1163, #10756, .T. ) ;
#10155 = CIRCLE ( 'NONE', #8761, 6.080745460913608902 ) ;
#10156 = FACE_OUTER_BOUND ( 'NONE', #7225, .T. ) ;
#10157 = LINE ( 'NONE', #6411, #816 ) ;
#10158 = LINE ( 'NONE', #5479, #2434 ) ;
#10159 = CARTESIAN_POINT ( 'NONE',  ( 4.999999999999999112, 0.000000000000000000, 0.000000000000000000 ) ) ;
#10160 = ORIENTED_EDGE ( 'NONE', *, *, #9260, .T. ) ;
#10161 = DIRECTION ( 'NONE',  ( -1.000000000000000000, -0.000000000000000000, -0.000000000000000000 ) ) ;
#10162 = ORIENTED_EDGE ( 'NONE', *, *, #4195, .T. ) ;
#10163 = DIRECTION ( 'NONE',  ( 1.387778780781445676E-17, 0.7900737791495476836, 0.6130117645692875206 ) ) ;
#10164 = ORIENTED_EDGE ( 'NONE', *, *, #6372, .T. ) ;
#10165 = FACE_OUTER_BOUND ( 'NONE', #1672, .T. ) ;
#10166 = CIRCLE ( 'NONE', #4772, 7.500000000000000888 ) ;
#10167 = DIRECTION ( 'NONE',  ( 0.000000000000000000, 0.000000000000000000, -1.000000000000000000 ) ) ;
#10168 = ORIENTED_EDGE ( 'NONE', *, *, #4376, .T. ) ;
#10169 = DIRECTION ( 'NONE',  ( 0.000000000000000000, 0.000000000000000000, -1.000000000000000000 ) ) ;
#10170 = AXIS2_PLACEMENT_3D ( 'NONE', #1957, #8655, #3711 ) ;
#10171 = CIRCLE ( 'NONE', #3591, 2.500000000000002220 ) ;
#10172 = ORIENTED_EDGE ( 'NONE', *, *, #10879, .F. ) ;
#10173 = AXIS2_PLACEMENT_3D ( 'NONE', #12237, #2738, #4687 ) ;
#10174 = CARTESIAN_POINT ( 'NONE',  ( 0.000000000000000000, -22.37914155802283034, -2.791921004064479739 ) ) ;
#10175 = VERTEX_POINT ( 'NONE', #3201 ) ;
#10176 = CYLINDRICAL_SURFACE ( 'NONE', #904, 9.600000000009600853 ) ;
#10177 = EDGE_LOOP ( 'NONE', ( #11857, #9798, #11934, #10263 ) ) ;
#10178 = DIRECTION ( 'NONE',  ( -1.000000000000000000, -0.000000000000000000, 0.000000000000000000 ) ) ;
#10179 = EDGE_CURVE ( 'NONE', #3914, #7364, #12226, .T. ) ;
#10180 = AXIS2_PLACEMENT_3D ( 'NONE', #2255, #5185, #1310 ) ;
#10181 = CARTESIAN_POINT ( 'NONE',  ( 51.00000000000000000, 5.744562646538045492, -38.00000000000000000 ) ) ;
#10182 = DIRECTION ( 'NONE',  ( 0.000000000000000000, 0.000000000000000000, 1.000000000000000000 ) ) ;
#10183 = FACE_BOUND ( 'NONE', #8047, .T. ) ;
#10184 = CIRCLE ( 'NONE', #8409, 5.000000000000000000 ) ;
#10185 = EDGE_LOOP ( 'NONE', ( #9603, #1550, #8009, #6659 ) ) ;
#10186 = ORIENTED_EDGE ( 'NONE', *, *, #2867, .T. ) ;
#10187 = DIRECTION ( 'NONE',  ( 0.000000000000000000, 0.000000000000000000, 1.000000000000000000 ) ) ;
#10188 = AXIS2_PLACEMENT_3D ( 'NONE', #10421, #9017, #9433 ) ;
#10189 = DIRECTION ( 'NONE',  ( -1.000000000000000000, -0.000000000000000000, -0.000000000000000000 ) ) ;
#10190 = CIRCLE ( 'NONE', #5803, 21.00000000002100009 ) ;
#10191 = ORIENTED_EDGE ( 'NONE', *, *, #8267, .F. ) ;
#10192 = DIRECTION ( 'NONE',  ( 1.000000000000000000, -0.000000000000000000, -0.000000000000000000 ) ) ;
#10193 = EDGE_CURVE ( 'NONE', #4722, #9598, #6867, .T. ) ;
#10194 = ORIENTED_EDGE ( 'NONE', *, *, #8976, .T. ) ;
#10195 = CARTESIAN_POINT ( 'NONE',  ( 46.00000000000000000, 3.500000000000001332, -45.49999999999998579 ) ) ;
#10196 = EDGE_CURVE ( 'NONE', #10053, #7220, #2192, .T. ) ;
#10197 = EDGE_CURVE ( 'NONE', #12260, #2345, #8455, .T. ) ;
#10198 = PRODUCT_DEFINITION_SHAPE ( 'NONE', 'NONE',  #7554 ) ;
#10199 = CIRCLE ( 'NONE', #5820, 20.24900000002025280 ) ;
#10200 = CIRCLE ( 'NONE', #3013, 7.200000000007202416 ) ;
#10201 = FILL_AREA_STYLE_COLOUR ( '', #4996 ) ;
#10202 = DIRECTION ( 'NONE',  ( 1.000000000000000000, 0.000000000000000000, 0.000000000000000000 ) ) ;
#10203 = CARTESIAN_POINT ( 'NONE',  ( 0.000000000000000000, 0.5999999999999998668, 2.622672778259560467 ) ) ;
#10204 = DIRECTION ( 'NONE',  ( -1.000000000000000000, -0.000000000000000000, -0.000000000000000000 ) ) ;
#10205 = ORIENTED_EDGE ( 'NONE', *, *, #11724, .F. ) ;
#10206 = CYLINDRICAL_SURFACE ( 'NONE', #10949, 27.00000000002699707 ) ;
#10207 = DIRECTION ( 'NONE',  ( -1.000000000000000000, -0.000000000000000000, 0.000000000000000000 ) ) ;
#10208 = PRESENTATION_LAYER_ASSIGNMENT (  '', '', ( #4626 ) ) ;
#10209 = AXIS2_PLACEMENT_3D ( 'NONE', #2979, #8736, #9801 ) ;
#10210 = EDGE_LOOP ( 'NONE', ( #6042, #11645 ) ) ;
#10211 = CARTESIAN_POINT ( 'NONE',  ( 4.999999999999999112, 6.283573709965309284, 19.24938187143298052 ) ) ;
#10212 = CIRCLE ( 'NONE', #11610, 21.00000000002100009 ) ;
#10213 = ORIENTED_EDGE ( 'NONE', *, *, #11975, .T. ) ;
#10214 = VECTOR ( 'NONE', #9747, 1000.000000000000000 ) ;
#10215 = ADVANCED_FACE ( 'NONE', ( #2311, #9946, #3374 ), #5128, .T. ) ;
#10216 = ADVANCED_FACE ( 'NONE', ( #7083 ), #5075, .T. ) ;
#10217 = EDGE_CURVE ( 'NONE', #1460, #5429, #9325, .T. ) ;
#10218 = DIRECTION ( 'NONE',  ( 0.000000000000000000, 0.000000000000000000, 1.000000000000000000 ) ) ;
#10219 =( GEOMETRIC_REPRESENTATION_CONTEXT ( 3 ) GLOBAL_UNCERTAINTY_ASSIGNED_CONTEXT ( ( #3767 ) ) GLOBAL_UNIT_ASSIGNED_CONTEXT ( ( #4615, #8503, #4547 ) ) REPRESENTATION_CONTEXT ( 'NONE', 'WORKASPACE' ) );
#10220 = CARTESIAN_POINT ( 'NONE',  ( 4.999999999999999112, -18.05452603534171985, 9.168210874537514599 ) ) ;
#10221 = DIRECTION ( 'NONE',  ( -1.000000000000000000, 0.000000000000000000, -0.000000000000000000 ) ) ;
#10222 = CIRCLE ( 'NONE', #8635, 2.500000000000000444 ) ;
#10223 = CARTESIAN_POINT ( 'NONE',  ( 15.00000000000000355, 30.00000000000000711, -1.999999999999998224 ) ) ;
#10224 = DIRECTION ( 'NONE',  ( 1.000000000000000000, 0.000000000000000000, 0.000000000000000000 ) ) ;
#10225 = ORIENTED_EDGE ( 'NONE', *, *, #7988, .F. ) ;
#10226 = LINE ( 'NONE', #8349, #5648 ) ;
#10227 = VERTEX_POINT ( 'NONE', #6507 ) ;
#10228 = DIRECTION ( 'NONE',  ( 0.000000000000000000, 0.000000000000000000, -1.000000000000000000 ) ) ;
#10229 = ADVANCED_FACE ( 'NONE', ( #3448 ), #8378, .F. ) ;
#10231 = EDGE_CURVE ( 'NONE', #1934, #5929, #2440, .T. ) ;
#10230 = ORIENTED_EDGE ( 'NONE', *, *, #12044, .T. ) ;
#10232 = PRODUCT_DEFINITION_FORMATION_WITH_SPECIFIED_SOURCE ( 'ANY', '', #6127, .NOT_KNOWN. ) ;
#10233 = AXIS2_PLACEMENT_3D ( 'NONE', #6718, #2017, #10512 ) ;
#10234 = AXIS2_PLACEMENT_3D ( 'NONE', #2937, #6755, #2002 ) ;
#10235 = CYLINDRICAL_SURFACE ( 'NONE', #1164, 12.49999999999999645 ) ;
#10236 = ORIENTED_EDGE ( 'NONE', *, *, #4554, .F. ) ;
#10237 = DIRECTION ( 'NONE',  ( 1.000000000000000000, 0.000000000000000000, 0.000000000000000000 ) ) ;
#10238 = AXIS2_PLACEMENT_3D ( 'NONE', #10647, #2081, #5705 ) ;
#10239 = VERTEX_POINT ( 'NONE', #10307 ) ;
#10240 = AXIS2_PLACEMENT_3D ( 'NONE', #7277, #1561, #9272 ) ;
#10241 = DIRECTION ( 'NONE',  ( 0.000000000000000000, 0.000000000000000000, -1.000000000000000000 ) ) ;
#10242 = ORIENTED_EDGE ( 'NONE', *, *, #12293, .T. ) ;
#10243 = EDGE_CURVE ( 'NONE', #4464, #1857, #6054, .T. ) ;
#10244 = DIRECTION ( 'NONE',  ( 0.000000000000000000, 1.000000000000000000, -1.224646799147353207E-16 ) ) ;
#10245 = ORIENTED_EDGE ( 'NONE', *, *, #125, .F. ) ;
#10246 = DIRECTION ( 'NONE',  ( -1.000000000000000000, 0.000000000000000000, 0.000000000000000000 ) ) ;
#10247 = AXIS2_PLACEMENT_3D ( 'NONE', #1782, #9420, #4670 ) ;
#10248 = DIRECTION ( 'NONE',  ( 0.000000000000000000, 0.000000000000000000, 1.000000000000000000 ) ) ;
#10249 = CARTESIAN_POINT ( 'NONE',  ( 51.00000000000000000, -3.499999999999998668, -45.49999999999998579 ) ) ;
#10250 = DIRECTION ( 'NONE',  ( -1.000000000000000000, -0.000000000000000000, 0.000000000000000000 ) ) ;
#10251 = EDGE_LOOP ( 'NONE', ( #211, #3769, #2054, #4812 ) ) ;
#10252 = ORIENTED_EDGE ( 'NONE', *, *, #5802, .F. ) ;
#10253 = DIRECTION ( 'NONE',  ( 0.000000000000000000, 0.000000000000000000, 1.000000000000000000 ) ) ;
#10254 = CIRCLE ( 'NONE', #11848, 7.200000000007200640 ) ;
#10255 = CARTESIAN_POINT ( 'NONE',  ( 4.999999999999999112, 0.000000000000000000, 0.000000000000000000 ) ) ;
#10256 = CARTESIAN_POINT ( 'NONE',  ( 43.00000000000000000, 0.000000000000000000, 0.000000000000000000 ) ) ;
#10257 = ORIENTED_EDGE ( 'NONE', *, *, #4003, .F. ) ;
#10258 = CARTESIAN_POINT ( 'NONE',  ( 27.38165010660258503, 4.886001309506334600, -37.03844870997966154 ) ) ;
#10259 = CIRCLE ( 'NONE', #5086, 6.750000000000000000 ) ;
#10260 = DIRECTION ( 'NONE',  ( -1.000000000000000000, 0.000000000000000000, 0.000000000000000000 ) ) ;
#10261 = CARTESIAN_POINT ( 'NONE',  ( -1.500000000000001332, 0.000000000000000000, -5.750000000000000000 ) ) ;
#10262 = EDGE_CURVE ( 'NONE', #11408, #8402, #7660, .T. ) ;
#10263 = ORIENTED_EDGE ( 'NONE', *, *, #4246, .F. ) ;
#10264 = DIRECTION ( 'NONE',  ( 1.000000000000000000, 0.000000000000000000, 0.000000000000000000 ) ) ;
#10265 = DIRECTION ( 'NONE',  ( -0.000000000000000000, 1.000000000000000000, 0.000000000000000000 ) ) ;
#10266 = VERTEX_POINT ( 'NONE', #10249 ) ;
#10267 = ADVANCED_FACE ( 'NONE', ( #739 ), #12109, .T. ) ;
#10268 = DIRECTION ( 'NONE',  ( -1.000000000000000000, 0.000000000000000000, 0.000000000000000000 ) ) ;
#10269 = CARTESIAN_POINT ( 'NONE',  ( 0.000000000000000000, -1.178949249685213863, 2.042000000000002924 ) ) ;
#10270 = ORIENTED_EDGE ( 'NONE', *, *, #8882, .F. ) ;
#10271 = DIRECTION ( 'NONE',  ( 0.000000000000000000, 0.000000000000000000, -1.000000000000000000 ) ) ;
#10272 = VECTOR ( 'NONE', #6725, 1000.000000000000000 ) ;
#10273 = ORIENTED_EDGE ( 'NONE', *, *, #4888, .F. ) ;
#10274 = CARTESIAN_POINT ( 'NONE',  ( -0.2500000000000000000, -8.096141056083446585, -1.000000000000000000 ) ) ;
#10275 = CYLINDRICAL_SURFACE ( 'NONE', #7995, 6.080745460913608902 ) ;
#10276 = CYLINDRICAL_SURFACE ( 'NONE', #3621, 9.600000000009600853 ) ;
#10277 = EDGE_CURVE ( 'NONE', #9428, #11661, #3561, .T. ) ;
#10278 = AXIS2_PLACEMENT_3D ( 'NONE', #6570, #665, #10375 ) ;
#10279 = CARTESIAN_POINT ( 'NONE',  ( 0.000000000000000000, 4.769696007084728073, -1.500000000000000000 ) ) ;
#10280 = DIRECTION ( 'NONE',  ( -1.000000000000000000, 0.000000000000000000, 0.000000000000000000 ) ) ;
#10281 = ORIENTED_EDGE ( 'NONE', *, *, #12024, .F. ) ;
#10283 = EDGE_CURVE ( 'NONE', #4256, #11604, #7372, .T. ) ;
#10282 = ORIENTED_EDGE ( 'NONE', *, *, #10828, .T. ) ;
#10284 = ADVANCED_FACE ( 'NONE', ( #621 ), #5507, .T. ) ;
#10285 = CARTESIAN_POINT ( 'NONE',  ( 25.00000000000000000, 0.000000000000000000, 12.50000000000000000 ) ) ;
#10286 = EDGE_CURVE ( 'NONE', #7642, #4373, #175, .T. ) ;
#10287 = ORIENTED_EDGE ( 'NONE', *, *, #7796, .T. ) ;
#10288 = CARTESIAN_POINT ( 'NONE',  ( 4.999999999999999112, -11.14352537685188338, 19.60720892790249081 ) ) ;
#10289 = ORIENTED_EDGE ( 'NONE', *, *, #10071, .F. ) ;
#10290 = DIRECTION ( 'NONE',  ( 0.000000000000000000, 0.000000000000000000, 1.000000000000000000 ) ) ;
#10291 = LINE ( 'NONE', #2860, #2973 ) ;
#10292 = VERTEX_POINT ( 'NONE', #8449 ) ;
#10293 = CARTESIAN_POINT ( 'NONE',  ( 45.00000000000001421, 50.00000000000000711, -38.00000000000000000 ) ) ;
#10294 = ADVANCED_FACE ( 'NONE', ( #9197 ), #2550, .T. ) ;
#10295 = DIRECTION ( 'NONE',  ( 0.000000000000000000, 0.000000000000000000, 1.000000000000000000 ) ) ;
#10296 = EDGE_LOOP ( 'NONE', ( #378, #3451, #10205, #10472, #5560, #3344 ) ) ;
#10297 = DIRECTION ( 'NONE',  ( 0.000000000000000000, 0.000000000000000000, -1.000000000000000000 ) ) ;
#10298 = ORIENTED_EDGE ( 'NONE', *, *, #2333, .F. ) ;
#10299 = FILL_AREA_STYLE ('',( #925 ) ) ;
#10300 = DIRECTION ( 'NONE',  ( 0.000000000000000000, -1.000000000000000000, 0.000000000000000000 ) ) ;
#10301 = B_SPLINE_CURVE_WITH_KNOTS ( 'NONE', 3,
 ( #3372, #4610, #8193, #2865, #549, #496, #10352, #11293, #11419, #5316 ),
 .UNSPECIFIED., .F., .F.,
 ( 4, 2, 2, 2, 4 ),
 ( 0.004762249257309257751, 0.005185715735975977674, 0.005609182214642698464, 0.006032648693309418386, 0.006456115171976138309 ),
 .UNSPECIFIED. ) ;
#10302 = PRODUCT ( 'socket head cap screw_iso_ISO 4762 M5 x 12 - 12N', 'socket head cap screw_iso_ISO 4762 M5 x 12 - 12N', '', ( #3065 ) ) ;
#10303 = ORIENTED_EDGE ( 'NONE', *, *, #4945, .F. ) ;
#10304 = CARTESIAN_POINT ( 'NONE',  ( 76.00000000000000000, 46.00000000000001421, -41.99999999999999289 ) ) ;
#10305 = EDGE_CURVE ( 'NONE', #10589, #2426, #1166, .T. ) ;
#10306 = EDGE_CURVE ( 'NONE', #103, #5845, #11119, .T. ) ;
#10307 = CARTESIAN_POINT ( 'NONE',  ( 0.5590169943749478954, 0.000000000000000000, 6.750000000000000000 ) ) ;
#10308 = DIRECTION ( 'NONE',  ( 0.000000000000000000, 0.9238795325112876267, -0.3826834323650873393 ) ) ;
#10309 = VERTEX_POINT ( 'NONE', #11992 ) ;
#10310 = ORIENTED_EDGE ( 'NONE', *, *, #1367, .T. ) ;
#10311 = CARTESIAN_POINT ( 'NONE',  ( -20.63749999999999929, 6.123233995736766282E-16, 5.000000000000000000 ) ) ;
#10312 = CARTESIAN_POINT ( 'NONE',  ( 42.00000000000000000, 6.123233995736765296E-16, -5.000000000000000000 ) ) ;
#10313 = CARTESIAN_POINT ( 'NONE',  ( 4.999999999999999112, 16.90755573046746107, 6.716513609244568528 ) ) ;
#10314 = EDGE_LOOP ( 'NONE', ( #9242, #11793, #8511, #5857 ) ) ;
#10315 = DIRECTION ( 'NONE',  ( 0.000000000000000000, 0.000000000000000000, -1.000000000000000000 ) ) ;
#10316 =( REPRESENTATION_RELATIONSHIP ('NONE','NONE', #9709, #1953 ) REPRESENTATION_RELATIONSHIP_WITH_TRANSFORMATION ( #2969 )SHAPE_REPRESENTATION_RELATIONSHIP( ) );
#10317 = CARTESIAN_POINT ( 'NONE',  ( -25.00000000000000000, 3.061616997868383043E-15, -25.00000000000000000 ) ) ;
#10318 = FACE_OUTER_BOUND ( 'NONE', #6111, .T. ) ;
#10319 = VERTEX_POINT ( 'NONE', #4365 ) ;
#10320 = DIRECTION ( 'NONE',  ( 0.000000000000000000, -1.000000000000000000, 0.000000000000000000 ) ) ;
#10321 = DIRECTION ( 'NONE',  ( 1.000000000000000000, 0.000000000000000000, 0.000000000000000000 ) ) ;
#10322 = ORIENTED_EDGE ( 'NONE', *, *, #6010, .F. ) ;
#10323 = DIRECTION ( 'NONE',  ( 0.000000000000000000, 0.000000000000000000, 1.000000000000000000 ) ) ;
#10324 = FACE_OUTER_BOUND ( 'NONE', #4708, .T. ) ;
#10325 = EDGE_LOOP ( 'NONE', ( #4740, #11454, #3006, #4635 ) ) ;
#10326 = DIRECTION ( 'NONE',  ( -0.000000000000000000, 1.000000000000000000, 1.224646799147353207E-16 ) ) ;
#10327 = ORIENTED_EDGE ( 'NONE', *, *, #560, .T. ) ;
#10328 = EDGE_CURVE ( 'NONE', #5131, #5049, #12339, .T. ) ;
#10329 =( LENGTH_UNIT ( ) NAMED_UNIT ( * ) SI_UNIT ( .MILLI., .METRE. ) );
#10330 = CYLINDRICAL_SURFACE ( 'NONE', #2007, 20.24900000002024569 ) ;
#10331 = FACE_BOUND ( 'NONE', #5817, .T. ) ;
#10332 = LINE ( 'NONE', #768, #6239 ) ;
#10333 = DIRECTION ( 'NONE',  ( 0.000000000000000000, 0.000000000000000000, -1.000000000000000000 ) ) ;
#10334 = VERTEX_POINT ( 'NONE', #7449 ) ;
#10335 = ORIENTED_EDGE ( 'NONE', *, *, #8979, .F. ) ;
#10336 = FACE_OUTER_BOUND ( 'NONE', #7173, .T. ) ;
#10337 = ORIENTED_EDGE ( 'NONE', *, *, #11603, .T. ) ;
#10338 = CYLINDRICAL_SURFACE ( 'NONE', #10247, 9.600000000009600853 ) ;
#10339 = SHAPE_DEFINITION_REPRESENTATION ( #11609, #11292 ) ;
#10340 = ORIENTED_EDGE ( 'NONE', *, *, #10824, .F. ) ;
#10341 = DIRECTION ( 'NONE',  ( 0.000000000000000000, 0.000000000000000000, 1.000000000000000000 ) ) ;
#10342 = ADVANCED_FACE ( 'NONE', ( #1745 ), #9766, .T. ) ;
#10343 = DIRECTION ( 'NONE',  ( 0.000000000000000000, -0.5000000000000069944, 0.8660254037844344888 ) ) ;
#10344 = CIRCLE ( 'NONE', #2163, 5.000000000000004441 ) ;
#10345 = VECTOR ( 'NONE', #3814, 1000.000000000000000 ) ;
#10346 = EDGE_CURVE ( 'NONE', #8188, #908, #12238, .T. ) ;
#10347 = VERTEX_POINT ( 'NONE', #7567 ) ;
#10348 = AXIS2_PLACEMENT_3D ( 'NONE', #7215, #11936, #3338 ) ;
#10349 = EDGE_CURVE ( 'NONE', #7385, #3952, #10632, .T. ) ;
#10350 = EDGE_LOOP ( 'NONE', ( #9681, #4849, #4427, #6920 ) ) ;
#10351 = LINE ( 'NONE', #10293, #8210 ) ;
#10352 = CARTESIAN_POINT ( 'NONE',  ( 0.1192621039632846131, 0.5999999999999998668, 3.174418872716579187 ) ) ;
#10353 = CARTESIAN_POINT ( 'NONE',  ( 4.999999999999999112, 0.000000000000000000, 0.000000000000000000 ) ) ;
#10354 = ORIENTED_EDGE ( 'NONE', *, *, #1585, .F. ) ;
#10355 = LINE ( 'NONE', #8620, #2378 ) ;
#10356 = ORIENTED_EDGE ( 'NONE', *, *, #3548, .F. ) ;
#10357 = CIRCLE ( 'NONE', #3583, 4.799999999999998934 ) ;
#10358 = SURFACE_STYLE_USAGE ( .BOTH. , #3874 ) ;
#10359 = CLOSED_SHELL ( 'NONE', ( #4398, #2239, #10701, #1194, #7492, #8396, #9227, #5789, #7765, #7650, #2343, #6274, #5506, #9359, #12331, #9323, #5643, #10294, #3025, #10507, #11572, #8377, #5921, #11570, #7242, #10043, #2872, #4468, #11501, #6994, #8254, #4322, #1898, #1965, #11127, #5801, #7752, #2477, #9757, #8352, #9697, #11965, #7321, #3475, #7726, #4079, #2382, #1836, #5898, #7562, #3939, #11348, #7869, #6177, #2481, #9600, #6151, #9301, #5283, #365, #1048 ) ) ;
#10360 = DIRECTION ( 'NONE',  ( -1.000000000000000000, 0.000000000000000000, -0.000000000000000000 ) ) ;
#10361 = ORIENTED_EDGE ( 'NONE', *, *, #9293, .F. ) ;
#10362 = CARTESIAN_POINT ( 'NONE',  ( 0.000000000000000000, -8.035066368449101049, -14.88411597386737562 ) ) ;
#10363 = PRODUCT_RELATED_PRODUCT_CATEGORY ( 'part', '', ( #6836 ) ) ;
#10364 = AXIS2_PLACEMENT_3D ( 'NONE', #44, #104, #3976 ) ;
#10365 = VECTOR ( 'NONE', #9132, 1000.000000000000000 ) ;
#10366 = DIRECTION ( 'NONE',  ( 1.000000000000000000, 0.000000000000000000, 0.000000000000000000 ) ) ;
#10367 = AXIS2_PLACEMENT_3D ( 'NONE', #2152, #5976, #8164 ) ;
#10368 = CARTESIAN_POINT ( 'NONE',  ( 15.00000000000000355, 30.00000000000000711, 0.000000000000000000 ) ) ;
#10369 = DIRECTION ( 'NONE',  ( 0.000000000000000000, 0.000000000000000000, 1.000000000000000000 ) ) ;
#10370 = ORIENTED_EDGE ( 'NONE', *, *, #4095, .T. ) ;
#10371 = ORIENTED_EDGE ( 'NONE', *, *, #4149, .F. ) ;
#10372 = LINE ( 'NONE', #5511, #11841 ) ;
#10373 = CYLINDRICAL_SURFACE ( 'NONE', #12198, 21.00000000002100009 ) ;
#10374 = CIRCLE ( 'NONE', #10972, 6.080745460913608902 ) ;
#10375 = DIRECTION ( 'NONE',  ( 0.000000000000000000, -0.7071067811865536790, 0.7071067811865413555 ) ) ;
#10376 = EDGE_CURVE ( 'NONE', #6297, #5352, #9785, .T. ) ;
#10377 = ORIENTED_EDGE ( 'NONE', *, *, #8754, .F. ) ;
#10378 = CARTESIAN_POINT ( 'NONE',  ( -15.00000000000000000, 44.00000000000001421, -2.149999999999999023 ) ) ;
#10379 = EDGE_CURVE ( 'NONE', #777, #5674, #7565, .T. ) ;
#10380 = COLOUR_RGB ( '',0.8941176470588234615, 0.8941176470588234615, 0.8941176470588234615 ) ;
#10381 = VECTOR ( 'NONE', #8394, 1000.000000000000000 ) ;
#10382 = DIRECTION ( 'NONE',  ( -1.000000000000000000, -0.000000000000000000, 0.000000000000000000 ) ) ;
#10383 = DIRECTION ( 'NONE',  ( 1.000000000000000000, 0.000000000000000000, 0.000000000000000000 ) ) ;
#10384 = ORIENTED_EDGE ( 'NONE', *, *, #8782, .F. ) ;
#10385 = CIRCLE ( 'NONE', #10983, 9.600000000009602630 ) ;
#10386 = DIRECTION ( 'NONE',  ( -1.000000000000000000, 0.000000000000000000, -0.000000000000000000 ) ) ;
#10387 = CARTESIAN_POINT ( 'NONE',  ( 1.499999999999999778, 7.399999999999999467, 0.000000000000000000 ) ) ;
#10388 = ORIENTED_EDGE ( 'NONE', *, *, #4166, .T. ) ;
#10389 = CARTESIAN_POINT ( 'NONE',  ( 4.999999999999997335, 0.000000000000000000, 5.000000000000000000 ) ) ;
#10390 = FACE_BOUND ( 'NONE', #5179, .T. ) ;
#10391 = ORIENTED_EDGE ( 'NONE', *, *, #5937, .T. ) ;
#10392 = DIRECTION ( 'NONE',  ( 1.000000000000000000, -0.000000000000000000, -0.000000000000000000 ) ) ;
#10393 = UNCERTAINTY_MEASURE_WITH_UNIT (LENGTH_MEASURE( 1.000000000000000082E-05 ), #8003, 'distance_accuracy_value', 'NONE');
#10394 = ORIENTED_EDGE ( 'NONE', *, *, #2766, .T. ) ;
#10395 = VECTOR ( 'NONE', #9892, 1000.000000000000000 ) ;
#10396 = VECTOR ( 'NONE', #5796, 1000.000000000000000 ) ;
#10397 =( LENGTH_UNIT ( ) NAMED_UNIT ( * ) SI_UNIT ( .MILLI., .METRE. ) );
#10398 = DIRECTION ( 'NONE',  ( -1.000000000000000000, 0.000000000000000000, 0.000000000000000000 ) ) ;
#10399 = DIRECTION ( 'NONE',  ( 0.000000000000000000, 0.000000000000000000, -1.000000000000000000 ) ) ;
#10400 = DIRECTION ( 'NONE',  ( -1.000000000000000000, 0.000000000000000000, 0.000000000000000000 ) ) ;
#10401 = DIRECTION ( 'NONE',  ( -1.000000000000000000, -0.000000000000000000, -0.000000000000000000 ) ) ;
#10402 = AXIS2_PLACEMENT_3D ( 'NONE', #4975, #3866, #8802 ) ;
#10403 = EDGE_LOOP ( 'NONE', ( #3327, #176, #10672, #967 ) ) ;
#10404 = ORIENTED_EDGE ( 'NONE', *, *, #12293, .F. ) ;
#10405 = AXIS2_PLACEMENT_3D ( 'NONE', #6413, #11279, #12139 ) ;
#10406 = DIRECTION ( 'NONE',  ( 0.000000000000000000, 0.000000000000000000, -1.000000000000000000 ) ) ;
#10407 = AXIS2_PLACEMENT_3D ( 'NONE', #11720, #6060, #3929 ) ;
#10408 = ORIENTED_EDGE ( 'NONE', *, *, #3181, .F. ) ;
#10409 = PRODUCT_CONTEXT ( 'NONE', #2820, 'mechanical' ) ;
#10410 = ORIENTED_EDGE ( 'NONE', *, *, #1367, .F. ) ;
#10411 = DIRECTION ( 'NONE',  ( 0.000000000000000000, -1.000000000000000000, 0.000000000000000000 ) ) ;
#10412 = CYLINDRICAL_SURFACE ( 'NONE', #1772, 20.24900000002024569 ) ;
#10413 = CIRCLE ( 'NONE', #5840, 9.600000000009600853 ) ;
#10414 = AXIS2_PLACEMENT_3D ( 'NONE', #11508, #4832, #8657 ) ;
#10415 = VECTOR ( 'NONE', #9962, 1000.000000000000000 ) ;
#10416 = EDGE_LOOP ( 'NONE', ( #3024, #5250 ) ) ;
#10417 = AXIS2_PLACEMENT_3D ( 'NONE', #5085, #11756, #11880 ) ;
#10418 = VERTEX_POINT ( 'NONE', #7640 ) ;
#10419 = LINE ( 'NONE', #1866, #5605 ) ;
#10420 = DIRECTION ( 'NONE',  ( 2.817067928751547788E-17, 0.6371047110838219396, -0.7707772616747329275 ) ) ;
#10421 = CARTESIAN_POINT ( 'NONE',  ( 5.200000000000002842, 0.000000000000000000, 0.000000000000000000 ) ) ;
#10422 = EDGE_CURVE ( 'NONE', #7570, #7924, #8566, .T. ) ;
#10423 = EDGE_LOOP ( 'NONE', ( #5959, #2731, #2231, #8397 ) ) ;
#10424 = DIRECTION ( 'NONE',  ( 0.000000000000000000, 0.000000000000000000, -1.000000000000000000 ) ) ;
#10425 = AXIS2_PLACEMENT_3D ( 'NONE', #11317, #5645, #3648 ) ;
#10426 = ORIENTED_EDGE ( 'NONE', *, *, #7706, .T. ) ;
#10427 = AXIS2_PLACEMENT_3D ( 'NONE', #9006, #6945, #6069 ) ;
#10428 = EDGE_CURVE ( 'NONE', #3761, #4605, #3575, .T. ) ;
#10429 = AXIS2_PLACEMENT_3D ( 'NONE', #6398, #10204, #5397 ) ;
#10430 = ORIENTED_EDGE ( 'NONE', *, *, #2158, .T. ) ;
#10431 = LINE ( 'NONE', #8504, #5100 ) ;
#10432 = ORIENTED_EDGE ( 'NONE', *, *, #11883, .F. ) ;
#10433 = LINE ( 'NONE', #7698, #9165 ) ;
#10434 = PRODUCT_DEFINITION_FORMATION_WITH_SPECIFIED_SOURCE ( 'ANY', '', #330, .NOT_KNOWN. ) ;
#10435 = CIRCLE ( 'NONE', #7456, 7.500000000000000000 ) ;
#10436 = VECTOR ( 'NONE', #8792, 1000.000000000000000 ) ;
#10437 = CARTESIAN_POINT ( 'NONE',  ( 4.799999999999999822, 0.000000000000000000, -1.000000000000000000 ) ) ;
#10438 = AXIS2_PLACEMENT_3D ( 'NONE', #2134, #9770, #1193 ) ;
#10439 = LINE ( 'NONE', #6822, #5967 ) ;
#10440 = DIRECTION ( 'NONE',  ( 0.000000000000000000, 0.000000000000000000, 1.000000000000000000 ) ) ;
#10441 = ORIENTED_EDGE ( 'NONE', *, *, #5343, .F. ) ;
#10442 = ORIENTED_EDGE ( 'NONE', *, *, #1256, .T. ) ;
#10443 = DIRECTION ( 'NONE',  ( 1.000000000000000000, 0.000000000000000000, 0.000000000000000000 ) ) ;
#10444 = EDGE_CURVE ( 'NONE', #10027, #629, #2364, .T. ) ;
#10445 = APPLICATION_PROTOCOL_DEFINITION ( 'draft international standard', 'automotive_design', 1998, #4738 ) ;
#10446 = DIRECTION ( 'NONE',  ( -1.000000000000000000, 0.000000000000000000, 0.000000000000000000 ) ) ;
#10447 = EDGE_CURVE ( 'NONE', #1740, #11007, #3747, .T. ) ;
#10448 = ADVANCED_FACE ( 'NONE', ( #12298 ), #2805, .F. ) ;
#10449 = LINE ( 'NONE', #4818, #4900 ) ;
#10450 = AXIS2_PLACEMENT_3D ( 'NONE', #7203, #4258, #1509 ) ;
#10451 = ORIENTED_EDGE ( 'NONE', *, *, #1680, .T. ) ;
#10452 = CARTESIAN_POINT ( 'NONE',  ( -20.63749999999999929, 0.000000000000000000, 0.000000000000000000 ) ) ;
#10453 = CARTESIAN_POINT ( 'NONE',  ( -20.00000000000000000, 44.00000000000001421, 12.50000000000000000 ) ) ;
#10454 = CYLINDRICAL_SURFACE ( 'NONE', #1815, 27.00000000002699707 ) ;
#10455 = ADVANCED_FACE ( 'NONE', ( #2936, #7754 ), #10498, .F. ) ;
#10456 = CIRCLE ( 'NONE', #4867, 2.500000000000000444 ) ;
#10457 = LINE ( 'NONE', #3014, #4855 ) ;
#10458 = DIRECTION ( 'NONE',  ( 1.000000000000000000, 0.000000000000000000, 0.000000000000000000 ) ) ;
#10459 = VERTEX_POINT ( 'NONE', #931 ) ;
#10460 = CARTESIAN_POINT ( 'NONE',  ( 0.000000000000000000, 14.88411597386740404, -8.035066368449049534 ) ) ;
#10461 = CYLINDRICAL_SURFACE ( 'NONE', #2035, 5.000000000000000000 ) ;
#10462 = ORIENTED_EDGE ( 'NONE', *, *, #11295, .T. ) ;
#10463 = CARTESIAN_POINT ( 'NONE',  ( 2.499999999999999556, 20.41639017900859443, 4.916402349214656020 ) ) ;
#10464 = ORIENTED_EDGE ( 'NONE', *, *, #9578, .T. ) ;
#10465 = CIRCLE ( 'NONE', #3679, 9.600000000009602630 ) ;
#10466 = CARTESIAN_POINT ( 'NONE',  ( 15.00000000000000355, 40.00000000000000711, 1.999999999999998224 ) ) ;
#10467 = LINE ( 'NONE', #3961, #9561 ) ;
#10468 = ADVANCED_FACE ( 'NONE', ( #2001 ), #9452, .T. ) ;
#10469 = CARTESIAN_POINT ( 'NONE',  ( 0.000000000000000000, -14.46592441914974714, 15.22291137398917193 ) ) ;
#10470 = DIRECTION ( 'NONE',  ( 1.000000000000000000, 0.000000000000000000, 0.000000000000000000 ) ) ;
#10471 = ORIENTED_EDGE ( 'NONE', *, *, #2613, .T. ) ;
#10472 = ORIENTED_EDGE ( 'NONE', *, *, #7216, .F. ) ;
#10473 = LINE ( 'NONE', #7355, #9256 ) ;
#10474 = VERTEX_POINT ( 'NONE', #11304 ) ;
#10475 = APPLICATION_PROTOCOL_DEFINITION ( 'draft international standard', 'automotive_design', 1998, #3934 ) ;
#10476 = ORIENTED_EDGE ( 'NONE', *, *, #11568, .T. ) ;
#10477 = CARTESIAN_POINT ( 'NONE',  ( -25.39999999999996305, 0.000000000000000000, 0.000000000000000000 ) ) ;
#10478 = LINE ( 'NONE', #4540, #3369 ) ;
#10479 = AXIS2_PLACEMENT_3D ( 'NONE', #4451, #11186, #3514 ) ;
#10480 = ORIENTED_EDGE ( 'NONE', *, *, #10508, .T. ) ;
#10481 = VERTEX_POINT ( 'NONE', #11436 ) ;
#10482 = DIRECTION ( 'NONE',  ( 0.000000000000000000, 0.000000000000000000, 1.000000000000000000 ) ) ;
#10483 = CARTESIAN_POINT ( 'NONE',  ( 45.00000000000001421, 7.000000000000004441, -41.99999999999998579 ) ) ;
#10484 = CARTESIAN_POINT ( 'NONE',  ( 42.00000000000000000, -3.058102613202345665, 3.699730856038719207 ) ) ;
#10485 = CYLINDRICAL_SURFACE ( 'NONE', #8225, 21.00000000002100009 ) ;
#10486 = ORIENTED_EDGE ( 'NONE', *, *, #7462, .F. ) ;
#10487 = DIRECTION ( 'NONE',  ( -1.000000000000000000, -1.734723475976807094E-16, 0.000000000000000000 ) ) ;
#10488 = ORIENTED_EDGE ( 'NONE', *, *, #8557, .T. ) ;
#10489 = APPLICATION_CONTEXT ( 'automotive_design' ) ;
#10490 = CIRCLE ( 'NONE', #9108, 5.000000000000000000 ) ;
#10491 = EDGE_LOOP ( 'NONE', ( #10514, #7423, #5298, #1015, #2541, #4593, #10115, #3429, #8850, #1043, #1735, #9011, #7337, #9289, #1295, #2706, #9399, #10991, #3918, #3838, #10837, #6350, #7469, #7315, #7074, #1153, #7676, #9316, #7732, #95, #697, #6115, #157, #6258, #1316, #6383, #4685, #6790, #7466, #6987, #6344, #9631, #9571, #11352, #6957, #7359, #13, #10486, #12341, #9717, #5841, #10758, #9731, #2777, #10081, #7905, #9729, #6748, #43, #4797, #6386, #3669, #6601, #9516, #3693, #9199, #6553, #10601, #9674 ) ) ;
#10492 = CARTESIAN_POINT ( 'NONE',  ( 0.000000000000000000, 0.000000000000000000, -12.50000000000000000 ) ) ;
#10493 = ORIENTED_EDGE ( 'NONE', *, *, #4809, .F. ) ;
#10494 = CARTESIAN_POINT ( 'NONE',  ( 46.00000000000000000, -3.499999999999998668, -45.49999999999998579 ) ) ;
#10495 = ADVANCED_FACE ( 'NONE', ( #9641 ), #1067, .T. ) ;
#10496 = CARTESIAN_POINT ( 'NONE',  ( 45.00000000000000000, -2.263420294706659952, 4.458354917400590089 ) ) ;
#10497 = EDGE_CURVE ( 'NONE', #6597, #9430, #5767, .T. ) ;
#10498 = PLANE ( 'NONE',  #11340 ) ;
#10499 = FACE_OUTER_BOUND ( 'NONE', #6621, .T. ) ;
#10500 = EDGE_LOOP ( 'NONE', ( #11873, #10252, #6252, #3367 ) ) ;
#10501 = DIRECTION ( 'NONE',  ( 0.000000000000000000, 0.000000000000000000, 1.000000000000000000 ) ) ;
#10502 =( NAMED_UNIT ( * ) PLANE_ANGLE_UNIT ( ) SI_UNIT ( $, .RADIAN. ) );
#10503 = LINE ( 'NONE', #8573, #6445 ) ;
#10504 = CARTESIAN_POINT ( 'NONE',  ( 0.000000000000000000, -18.05452603534159195, -9.168210874537770394 ) ) ;
#10505 = ORIENTED_EDGE ( 'NONE', *, *, #366, .F. ) ;
#10506 = CARTESIAN_POINT ( 'NONE',  ( 0.000000000000000000, 0.000000000000000000, 0.000000000000000000 ) ) ;
#10507 = ADVANCED_FACE ( 'NONE', ( #3937 ), #4689, .T. ) ;
#10508 = EDGE_CURVE ( 'NONE', #88, #344, #10439, .T. ) ;
#10509 = EDGE_CURVE ( 'NONE', #5923, #394, #6561, .T. ) ;
#10510 = CARTESIAN_POINT ( 'NONE',  ( -31.74999999999995737, 0.000000000000000000, 0.000000000000000000 ) ) ;
#10511 = CARTESIAN_POINT ( 'NONE',  ( 26.00000000000000355, -12.50000000000000000, -41.99999999999999289 ) ) ;
#10512 = DIRECTION ( 'NONE',  ( 0.000000000000000000, 0.000000000000000000, 1.000000000000000000 ) ) ;
#10513 = DIRECTION ( 'NONE',  ( -1.000000000000000000, 0.000000000000000000, 0.000000000000000000 ) ) ;
#10514 = ORIENTED_EDGE ( 'NONE', *, *, #11654, .F. ) ;
#10515 = CARTESIAN_POINT ( 'NONE',  ( 0.000000000000000000, 21.74405275335758247, 5.984728032765037398 ) ) ;
#10516 = DIRECTION ( 'NONE',  ( 0.000000000000000000, 0.000000000000000000, 1.000000000000000000 ) ) ;
#10517 = ORIENTED_EDGE ( 'NONE', *, *, #4936, .T. ) ;
#10518 = CARTESIAN_POINT ( 'NONE',  ( 2.499999999999999556, -22.05152472667140984, 15.57980286237464895 ) ) ;
#10519 = UNCERTAINTY_MEASURE_WITH_UNIT (LENGTH_MEASURE( 1.000000000000000082E-05 ), #10862, 'distance_accuracy_value', 'NONE');
#10520 = ORIENTED_EDGE ( 'NONE', *, *, #11650, .T. ) ;
#10521 = CARTESIAN_POINT ( 'NONE',  ( 51.00000000000000000, 3.500000000000001332, -38.49999999999998579 ) ) ;
#10522 = EDGE_CURVE ( 'NONE', #10459, #3361, #6968, .T. ) ;
#10523 = CARTESIAN_POINT ( 'NONE',  ( -10.00000000000000000, 0.000000000000000000, 0.000000000000000000 ) ) ;
#10524 = DIRECTION ( 'NONE',  ( 0.000000000000000000, 0.000000000000000000, -1.000000000000000000 ) ) ;
#10525 = DIRECTION ( 'NONE',  ( -1.000000000000000000, -0.000000000000000000, -0.000000000000000000 ) ) ;
#10526 = CARTESIAN_POINT ( 'NONE',  ( 0.000000000000000000, 4.769696007084728073, 1.500000000000000000 ) ) ;
#10527 = ORIENTED_EDGE ( 'NONE', *, *, #4860, .F. ) ;
#10528 = ORIENTED_EDGE ( 'NONE', *, *, #3642, .F. ) ;
#10529 = DIRECTION ( 'NONE',  ( 1.000000000000000000, -0.000000000000000000, -0.000000000000000000 ) ) ;
#10530 = ORIENTED_EDGE ( 'NONE', *, *, #7865, .F. ) ;
#10531 = CARTESIAN_POINT ( 'NONE',  ( 0.000000000000000000, 0.000000000000000000, 0.000000000000000000 ) ) ;
#10532 = ITEM_DEFINED_TRANSFORMATION ( 'NONE', 'NONE', #11629,  #6056 ) ;
#10533 = ORIENTED_EDGE ( 'NONE', *, *, #11974, .T. ) ;
#10534 = EDGE_CURVE ( 'NONE', #972, #10913, #169, .T. ) ;
#10535 = EDGE_CURVE ( 'NONE', #3677, #1217, #9076, .T. ) ;
#10536 = ORIENTED_EDGE ( 'NONE', *, *, #6794, .T. ) ;
#10537 = ORIENTED_EDGE ( 'NONE', *, *, #8478, .T. ) ;
#10538 = LINE ( 'NONE', #2863, #778 ) ;
#10539 = DIRECTION ( 'NONE',  ( -0.000000000000000000, -0.000000000000000000, 1.000000000000000000 ) ) ;
#10540 = CARTESIAN_POINT ( 'NONE',  ( 0.000000000000000000, 0.000000000000000000, 0.000000000000000000 ) ) ;
#10541 = DIRECTION ( 'NONE',  ( 0.000000000000000000, 0.000000000000000000, 1.000000000000000000 ) ) ;
#10542 = ORIENTED_EDGE ( 'NONE', *, *, #5526, .T. ) ;
#10543 = DIRECTION ( 'NONE',  ( 1.000000000000000000, 0.000000000000000000, 0.000000000000000000 ) ) ;
#10544 = VERTEX_POINT ( 'NONE', #3313 ) ;
#10545 =( NAMED_UNIT ( * ) PLANE_ANGLE_UNIT ( ) SI_UNIT ( $, .RADIAN. ) );
#10546 = ORIENTED_EDGE ( 'NONE', *, *, #485, .F. ) ;
#10548 = CARTESIAN_POINT ( 'NONE',  ( 37.00000000000000711, -4.104405154062230115E-16, -2.224720805914714718E-17 ) ) ;
#10547 = AXIS2_PLACEMENT_3D ( 'NONE', #492, #4301, #11062 ) ;
#10549 = VERTEX_POINT ( 'NONE', #4064 ) ;
#10550 = DIRECTION ( 'NONE',  ( 1.000000000000000000, -0.000000000000000000, -0.000000000000000000 ) ) ;
#10551 = VECTOR ( 'NONE', #9039, 1000.000000000000000 ) ;
#10552 = DIRECTION ( 'NONE',  ( -1.000000000000000000, -0.000000000000000000, 0.000000000000000000 ) ) ;
#10553 = VECTOR ( 'NONE', #2932, 1000.000000000000000 ) ;
#10554 = VECTOR ( 'NONE', #7888, 1000.000000000000000 ) ;
#10555 = CARTESIAN_POINT ( 'NONE',  ( -26.00000000000000355, 0.000000000000000000, 0.000000000000000000 ) ) ;
#10556 = CARTESIAN_POINT ( 'NONE',  ( 0.000000000000000000, -5.950465759858725612, -20.13931372320394786 ) ) ;
#10557 = ORIENTED_EDGE ( 'NONE', *, *, #1332, .T. ) ;
#10558 = DIRECTION ( 'NONE',  ( -1.000000000000000000, -0.000000000000000000, -0.000000000000000000 ) ) ;
#10559 = FILL_AREA_STYLE ('',( #11309 ) ) ;
#10560 = DIRECTION ( 'NONE',  ( 0.000000000000000000, 0.000000000000000000, 1.000000000000000000 ) ) ;
#10561 = DIRECTION ( 'NONE',  ( -1.000000000000000000, 0.000000000000000000, 0.000000000000000000 ) ) ;
#10562 = ADVANCED_FACE ( 'NONE', ( #6996 ), #3768, .T. ) ;
#10563 = SHAPE_REPRESENTATION ( 'spur gear_iso_ISO - Spur gear 3M 16T 20PA 5FW ---S16A75H50L10.0S1', ( #6056 ), #3048 ) ;
#10564 = ORIENTED_EDGE ( 'NONE', *, *, #5544, .F. ) ;
#10565 = LINE ( 'NONE', #9572, #1998 ) ;
#10566 = CIRCLE ( 'NONE', #7577, 14.24900000001425049 ) ;
#10567 = CLOSED_SHELL ( 'NONE', ( #431, #9971, #8291, #1908, #4304, #11324, #12322, #6163, #412, #10748, #35, #1895, #1140, #10722, #1077, #8524, #1991, #8113, #4611, #5231, #8414, #3880 ) ) ;
#10568 = DIRECTION ( 'NONE',  ( 0.000000000000000000, 0.000000000000000000, -1.000000000000000000 ) ) ;
#10569 = DIRECTION ( 'NONE',  ( 0.000000000000000000, 0.000000000000000000, 1.000000000000000000 ) ) ;
#10570 = CYLINDRICAL_SURFACE ( 'NONE', #2857, 7.200000000007202416 ) ;
#10571 = FACE_OUTER_BOUND ( 'NONE', #4211, .T. ) ;
#10572 = CIRCLE ( 'NONE', #356, 9.600000000009600853 ) ;
#10573 = ORIENTED_EDGE ( 'NONE', *, *, #11723, .T. ) ;
#10574 = EDGE_CURVE ( 'NONE', #5514, #9474, #10922, .T. ) ;
#10575 = DIRECTION ( 'NONE',  ( 0.000000000000000000, 0.000000000000000000, -1.000000000000000000 ) ) ;
#10576 = CARTESIAN_POINT ( 'NONE',  ( 4.999999999999999112, -20.41639017900856246, -4.916402349214799017 ) ) ;
#10577 = CIRCLE ( 'NONE', #201, 20.24900000002024569 ) ;
#10578 = ORIENTED_EDGE ( 'NONE', *, *, #7462, .T. ) ;
#10579 = DIRECTION ( 'NONE',  ( -1.000000000000000000, -0.000000000000000000, 0.000000000000000000 ) ) ;
#10580 = EDGE_CURVE ( 'NONE', #8484, #3527, #11543, .T. ) ;
#10581 = EDGE_LOOP ( 'NONE', ( #8883, #11404, #9494, #7368 ) ) ;
#10582 = ADVANCED_FACE ( 'NONE', ( #9753 ), #11681, .T. ) ;
#10583 = AXIS2_PLACEMENT_3D ( 'NONE', #4217, #11955, #470 ) ;
#10584 = VECTOR ( 'NONE', #5886, 1000.000000000000000 ) ;
#10585 = CARTESIAN_POINT ( 'NONE',  ( 0.000000000000000000, 6.799999999999999822, -1.500000000000000000 ) ) ;
#10586 = FACE_OUTER_BOUND ( 'NONE', #8052, .T. ) ;
#10587 = CARTESIAN_POINT ( 'NONE',  ( -20.00000000000000000, 0.000000000000000000, 25.00000000000000000 ) ) ;
#10588 = DIRECTION ( 'NONE',  ( -1.000000000000000000, 0.000000000000000000, 0.000000000000000000 ) ) ;
#10589 = VERTEX_POINT ( 'NONE', #2243 ) ;
#10590 = ORIENTED_EDGE ( 'NONE', *, *, #2207, .T. ) ;
#10591 = VECTOR ( 'NONE', #19, 1000.000000000000000 ) ;
#10592 = ORIENTED_EDGE ( 'NONE', *, *, #9149, .T. ) ;
#10593 = LINE ( 'NONE', #11405, #12050 ) ;
#10594 = EDGE_CURVE ( 'NONE', #2589, #10481, #1768, .T. ) ;
#10595 = CONTEXT_DEPENDENT_SHAPE_REPRESENTATION ( #2656, #3442 ) ;
#10596 = CIRCLE ( 'NONE', #216, 7.000000000000006217 ) ;
#10597 = EDGE_CURVE ( 'NONE', #11181, #9643, #3132, .T. ) ;
#10598 = ORIENTED_EDGE ( 'NONE', *, *, #11777, .F. ) ;
#10599 = CIRCLE ( 'NONE', #6616, 5.000000000000004441 ) ;
#10600 = EDGE_CURVE ( 'NONE', #1066, #11750, #4767, .T. ) ;
#10601 = ORIENTED_EDGE ( 'NONE', *, *, #3739, .F. ) ;
#10602 = AXIS2_PLACEMENT_3D ( 'NONE', #260, #11741, #4073 ) ;
#10603 = ORIENTED_EDGE ( 'NONE', *, *, #4109, .T. ) ;
#10604 = AXIS2_PLACEMENT_3D ( 'NONE', #1958, #8842, #10516 ) ;
#10605 = DIRECTION ( 'NONE',  ( -1.000000000000000000, -0.000000000000000000, -0.000000000000000000 ) ) ;
#10606 = PLANE ( 'NONE',  #1009 ) ;
#10607 = AXIS2_PLACEMENT_3D ( 'NONE', #8118, #3236, #11715 ) ;
#10608 = AXIS2_PLACEMENT_3D ( 'NONE', #5411, #11277, #9348 ) ;
#10609 = VECTOR ( 'NONE', #11288, 1000.000000000000000 ) ;
#10610 = CARTESIAN_POINT ( 'NONE',  ( 2.500000000000000000, -1.178949249685213863, 2.042000000000002924 ) ) ;
#10611 = DIRECTION ( 'NONE',  ( 1.000000000000000000, -0.000000000000000000, -0.000000000000000000 ) ) ;
#10612 = ORIENTED_EDGE ( 'NONE', *, *, #12280, .T. ) ;
#10613 = EDGE_CURVE ( 'NONE', #4341, #4349, #5116, .T. ) ;
#10614 = EDGE_CURVE ( 'NONE', #7044, #5044, #8941, .T. ) ;
#10615 = CARTESIAN_POINT ( 'NONE',  ( 4.999999999999999112, 0.000000000000000000, 0.000000000000000000 ) ) ;
#10616 = ORIENTED_EDGE ( 'NONE', *, *, #8631, .F. ) ;
#10617 = ORIENTED_EDGE ( 'NONE', *, *, #8976, .F. ) ;
#10618 =( GEOMETRIC_REPRESENTATION_CONTEXT ( 3 ) GLOBAL_UNCERTAINTY_ASSIGNED_CONTEXT ( ( #1655 ) ) GLOBAL_UNIT_ASSIGNED_CONTEXT ( ( #6454, #1694, #6380 ) ) REPRESENTATION_CONTEXT ( 'NONE', 'WORKASPACE' ) );
#10619 = VECTOR ( 'NONE', #3407, 1000.000000000000000 ) ;
#10620 = FACE_OUTER_BOUND ( 'NONE', #1117, .T. ) ;
#10621 = VECTOR ( 'NONE', #694, 1000.000000000000000 ) ;
#10622 = PRODUCT_DEFINITION_SHAPE ( 'NONE', 'NONE',  #2198 ) ;
#10623 = CIRCLE ( 'NONE', #5031, 12.50000000000000000 ) ;
#10624 = ORIENTED_EDGE ( 'NONE', *, *, #6406, .T. ) ;
#10625 = CARTESIAN_POINT ( 'NONE',  ( -20.00000000000000000, 0.000000000000000000, 0.000000000000000000 ) ) ;
#10626 = CYLINDRICAL_SURFACE ( 'NONE', #5195, 5.000000000000004441 ) ;
#10627 = VECTOR ( 'NONE', #905, 1000.000000000000000 ) ;
#10628 = CIRCLE ( 'NONE', #1057, 21.00000000002100009 ) ;
#10629 = ORIENTED_EDGE ( 'NONE', *, *, #8547, .F. ) ;
#10630 = EDGE_CURVE ( 'NONE', #138, #11506, #6777, .T. ) ;
#10631 = CIRCLE ( 'NONE', #5239, 14.24900000001425227 ) ;
#10632 = LINE ( 'NONE', #2880, #1980 ) ;
#10633 = CARTESIAN_POINT ( 'NONE',  ( 4.999999999999999112, 11.14352537685202016, -19.60720892790241265 ) ) ;
#10634 = ORIENTED_EDGE ( 'NONE', *, *, #1023, .T. ) ;
#10635 = CARTESIAN_POINT ( 'NONE',  ( 42.00000000000000000, 4.769696007084728073, -1.500000000000000444 ) ) ;
#10636 = SHAPE_DEFINITION_REPRESENTATION ( #9629, #9709 ) ;
#10637 = DIRECTION ( 'NONE',  ( -0.000000000000000000, 1.000000000000000000, -0.000000000000000000 ) ) ;
#10638 = DIRECTION ( 'NONE',  ( -1.000000000000000000, -0.000000000000000000, -0.000000000000000000 ) ) ;
#10639 = VERTEX_POINT ( 'NONE', #5997 ) ;
#10640 = PLANE ( 'NONE',  #8989 ) ;
#10641 = ORIENTED_EDGE ( 'NONE', *, *, #8994, .T. ) ;
#10642 = AXIS2_PLACEMENT_3D ( 'NONE', #10143, #1644, #1575 ) ;
#10643 = AXIS2_PLACEMENT_3D ( 'NONE', #1667, #8541, #3781 ) ;
#10644 = AXIS2_PLACEMENT_3D ( 'NONE', #6081, #263, #9947 ) ;
#10645 = CARTESIAN_POINT ( 'NONE',  ( 4.999999999999999112, -22.37914155802283034, -2.791921004064479739 ) ) ;
#10646 = PLANE ( 'NONE',  #3811 ) ;
#10647 = CARTESIAN_POINT ( 'NONE',  ( -25.00000000000000000, 0.000000000000000000, 0.000000000000000000 ) ) ;
#10648 = FACE_OUTER_BOUND ( 'NONE', #10350, .T. ) ;
#10649 = VECTOR ( 'NONE', #8768, 1000.000000000000000 ) ;
#10650 = ORIENTED_EDGE ( 'NONE', *, *, #8530, .T. ) ;
#10651 = LINE ( 'NONE', #6022, #383 ) ;
#10652 = CIRCLE ( 'NONE', #9461, 14.24900000001425227 ) ;
#10653 = FACE_OUTER_BOUND ( 'NONE', #9262, .T. ) ;
#10654 = VERTEX_POINT ( 'NONE', #9937 ) ;
#10655 = CARTESIAN_POINT ( 'NONE',  ( 0.000000000000000000, -20.41639017900856246, -4.916402349214799017 ) ) ;
#10656 = PRODUCT_DEFINITION_CONTEXT ( 'detailed design', #11588, 'design' ) ;
#10657 = ORIENTED_EDGE ( 'NONE', *, *, #5484, .T. ) ;
#10658 = EDGE_CURVE ( 'NONE', #477, #4908, #11151, .T. ) ;
#10659 = AXIS2_PLACEMENT_3D ( 'NONE', #6827, #7943, #4994 ) ;
#10660 = DIRECTION ( 'NONE',  ( 0.000000000000000000, 0.000000000000000000, 1.000000000000000000 ) ) ;
#10661 = DIRECTION ( 'NONE',  ( -1.000000000000000000, 0.000000000000000000, 0.000000000000000000 ) ) ;
#10662 = EDGE_CURVE ( 'NONE', #353, #8440, #6172, .T. ) ;
#10663 = LINE ( 'NONE', #5964, #10816 ) ;
#10664 = CARTESIAN_POINT ( 'NONE',  ( 4.999999999999999112, 8.035066368449204077, 14.88411597386731877 ) ) ;
#10665 = VERTEX_POINT ( 'NONE', #7067 ) ;
#10666 = DIRECTION ( 'NONE',  ( -1.000000000000000000, 0.000000000000000000, 0.000000000000000000 ) ) ;
#10667 = ORIENTED_EDGE ( 'NONE', *, *, #1027, .T. ) ;
#10668 = CARTESIAN_POINT ( 'NONE',  ( 4.999999999999999112, 0.000000000000000000, 0.000000000000000000 ) ) ;
#10669 = EDGE_LOOP ( 'NONE', ( #4692, #6726, #5935, #4509, #4226, #8452 ) ) ;
#10670 = EDGE_CURVE ( 'NONE', #10919, #6904, #7178, .T. ) ;
#10671 = CARTESIAN_POINT ( 'NONE',  ( 42.00000000000000000, -2.824006678639516377, 3.881363971466655904 ) ) ;
#10672 = ORIENTED_EDGE ( 'NONE', *, *, #2946, .T. ) ;
#10673 = DIRECTION ( 'NONE',  ( 1.000000000000000000, 0.000000000000000000, 0.000000000000000000 ) ) ;
#10674 = DIRECTION ( 'NONE',  ( 0.000000000000000000, 0.000000000000000000, -1.000000000000000000 ) ) ;
#10675 = ADVANCED_FACE ( 'NONE', ( #421 ), #11858, .T. ) ;
#10676 = EDGE_CURVE ( 'NONE', #10544, #4720, #11940, .T. ) ;
#10677 = LINE ( 'NONE', #106, #7819 ) ;
#10679 = EDGE_CURVE ( 'NONE', #8903, #3376, #6574, .T. ) ;
#10678 = CARTESIAN_POINT ( 'NONE',  ( 4.999999999999999112, 14.88411597386740404, -8.035066368449049534 ) ) ;
#10680 = ORIENTED_EDGE ( 'NONE', *, *, #6691, .T. ) ;
#10681 = PLANE ( 'NONE',  #11399 ) ;
#10682 = ORIENTED_EDGE ( 'NONE', *, *, #3195, .F. ) ;
#10683 = ORIENTED_EDGE ( 'NONE', *, *, #6301, .F. ) ;
#10684 = PLANE ( 'NONE',  #1826 ) ;
#10685 = CIRCLE ( 'NONE', #8492, 5.199999999999996625 ) ;
#10686 = ORIENTED_EDGE ( 'NONE', *, *, #11112, .T. ) ;
#10687 = DIRECTION ( 'NONE',  ( 0.000000000000000000, 0.000000000000000000, -1.000000000000000000 ) ) ;
#10688 = CARTESIAN_POINT ( 'NONE',  ( 0.000000000000000000, -15.22291137398912397, -14.46592441914980753 ) ) ;
#10689 = EDGE_LOOP ( 'NONE', ( #8956, #7748, #4682, #940 ) ) ;
#10690 = CIRCLE ( 'NONE', #5302, 4.799999999999999822 ) ;
#10691 = CARTESIAN_POINT ( 'NONE',  ( 0.000000000000000000, 0.000000000000000000, 0.000000000000000000 ) ) ;
#10692 = FACE_OUTER_BOUND ( 'NONE', #8175, .T. ) ;
#10693 = ORIENTED_EDGE ( 'NONE', *, *, #10890, .F. ) ;
#10694 = DIRECTION ( 'NONE',  ( 0.000000000000000000, 0.000000000000000000, 1.000000000000000000 ) ) ;
#10695 = SURFACE_SIDE_STYLE ('',( #6894 ) ) ;
#10696 = CYLINDRICAL_SURFACE ( 'NONE', #5444, 2.149999999999999023 ) ;
#10697 = CARTESIAN_POINT ( 'NONE',  ( 1.500000000000000888, 0.000000000000000000, -5.100000000000000533 ) ) ;
#10698 = ORIENTED_EDGE ( 'NONE', *, *, #3444, .F. ) ;
#10699 = DIRECTION ( 'NONE',  ( 1.000000000000000000, -0.000000000000000000, -0.000000000000000000 ) ) ;
#10700 = EDGE_CURVE ( 'NONE', #7142, #4908, #5432, .T. ) ;
#10701 = ADVANCED_FACE ( 'NONE', ( #1681 ), #732, .T. ) ;
#10702 = DIRECTION ( 'NONE',  ( 0.000000000000000000, 0.000000000000000000, -1.000000000000000000 ) ) ;
#10703 = DIRECTION ( 'NONE',  ( -1.000000000000000000, -0.000000000000000000, -0.000000000000000000 ) ) ;
#10704 = CARTESIAN_POINT ( 'NONE',  ( 51.00000000000000000, 46.00000000000001421, -46.00000000000000000 ) ) ;
#10705 = ORIENTED_EDGE ( 'NONE', *, *, #2650, .F. ) ;
#10706 = DIRECTION ( 'NONE',  ( 1.000000000000000000, 0.000000000000000000, 0.000000000000000000 ) ) ;
#10707 = DIRECTION ( 'NONE',  ( 1.000000000000000000, 0.000000000000000000, 0.000000000000000000 ) ) ;
#10708 = ORIENTED_EDGE ( 'NONE', *, *, #9696, .T. ) ;
#10709 = CARTESIAN_POINT ( 'NONE',  ( 37.00000000000000711, -4.210917358895616580, -2.303947698310783387 ) ) ;
#10710 = VERTEX_POINT ( 'NONE', #3362 ) ;
#10711 = CARTESIAN_POINT ( 'NONE',  ( 4.999999999999999112, 19.24938187143296275, 6.283573709965379450 ) ) ;
#10712 = DIRECTION ( 'NONE',  ( 0.000000000000000000, 0.000000000000000000, -1.000000000000000000 ) ) ;
#10713 = DIRECTION ( 'NONE',  ( 0.5150380737757255245, 1.049727191973305394E-16, 0.8571673013836856869 ) ) ;
#10714 = FACE_OUTER_BOUND ( 'NONE', #295, .T. ) ;
#10715 = DIRECTION ( 'NONE',  ( 0.000000000000000000, -0.000000000000000000, 1.000000000000000000 ) ) ;
#10716 = PRODUCT_DEFINITION_SHAPE ( 'NONE', 'NONE',  #12356 ) ;
#10717 = VERTEX_POINT ( 'NONE', #11239 ) ;
#10718 = FACE_OUTER_BOUND ( 'NONE', #4108, .T. ) ;
#10719 = ORIENTED_EDGE ( 'NONE', *, *, #7237, .F. ) ;
#10720 = FACE_OUTER_BOUND ( 'NONE', #10085, .T. ) ;
#10721 = ORIENTED_EDGE ( 'NONE', *, *, #3118, .T. ) ;
#10722 = ADVANCED_FACE ( 'NONE', ( #2424 ), #5309, .F. ) ;
#10723 = APPLICATION_CONTEXT ( 'automotive_design' ) ;
#10724 = DIRECTION ( 'NONE',  ( 0.1305261922200524338, -0.9914448613738102711, 0.000000000000000000 ) ) ;
#10725 = VERTEX_POINT ( 'NONE', #7436 ) ;
#10726 = DIRECTION ( 'NONE',  ( 1.000000000000000000, 0.000000000000000000, 0.000000000000000000 ) ) ;
#10727 = CARTESIAN_POINT ( 'NONE',  ( 0.8603238823369437904, 0.5999999999999998668, -3.802997805305113665 ) ) ;
#10728 = DIRECTION ( 'NONE',  ( 0.000000000000000000, 0.000000000000000000, -1.000000000000000000 ) ) ;
#10729 = CYLINDRICAL_SURFACE ( 'NONE', #4022, 24.99999999999998579 ) ;
#10730 = ORIENTED_EDGE ( 'NONE', *, *, #10059, .T. ) ;
#10731 = ORIENTED_EDGE ( 'NONE', *, *, #4539, .T. ) ;
#10732 = EDGE_CURVE ( 'NONE', #2996, #733, #2604, .T. ) ;
#10733 = ORIENTED_EDGE ( 'NONE', *, *, #7034, .F. ) ;
#10734 = CARTESIAN_POINT ( 'NONE',  ( 4.999999999999999112, 14.40062958310465469, -8.872489362018239234 ) ) ;
#10735 = EDGE_CURVE ( 'NONE', #709, #4941, #5172, .T. ) ;
#10736 = EDGE_LOOP ( 'NONE', ( #10404, #11383 ) ) ;
#10737 = CARTESIAN_POINT ( 'NONE',  ( 2.500000000000000000, 2.357898499370433054, -1.951563910473907981E-15 ) ) ;
#10738 = EDGE_CURVE ( 'NONE', #420, #4839, #2571, .T. ) ;
#10739 = LINE ( 'NONE', #8937, #2398 ) ;
#10740 = ORIENTED_EDGE ( 'NONE', *, *, #9033, .T. ) ;
#10741 = DIRECTION ( 'NONE',  ( -1.000000000000000000, 0.000000000000000000, 0.000000000000000000 ) ) ;
#10742 = DIRECTION ( 'NONE',  ( 0.000000000000000000, 0.000000000000000000, -1.000000000000000000 ) ) ;
#10743 = ORIENTED_EDGE ( 'NONE', *, *, #1493, .F. ) ;
#10744 = CARTESIAN_POINT ( 'NONE',  ( 51.00000000000000000, 0.000000000000000000, -44.50000000000000000 ) ) ;
#10745 = CARTESIAN_POINT ( 'NONE',  ( -25.39999999999996305, 2.449293598294706414E-16, -2.000000000000000000 ) ) ;
#10746 = VECTOR ( 'NONE', #276, 1000.000000000000000 ) ;
#10747 = CARTESIAN_POINT ( 'NONE',  ( 2.500000000000000000, -2.357898499370432610, 3.252606517456513302E-15 ) ) ;
#10748 = ADVANCED_FACE ( 'NONE', ( #8310 ), #4544, .T. ) ;
#10749 = ORIENTED_EDGE ( 'NONE', *, *, #10600, .T. ) ;
#10750 = DIRECTION ( 'NONE',  ( 0.000000000000000000, 0.000000000000000000, 1.000000000000000000 ) ) ;
#10751 = ADVANCED_FACE ( 'NONE', ( #12098 ), #9574, .T. ) ;
#10752 = VECTOR ( 'NONE', #301, 1000.000000000000000 ) ;
#10753 = AXIS2_PLACEMENT_3D ( 'NONE', #5913, #1209, #10895 ) ;
#10754 = DIRECTION ( 'NONE',  ( 0.000000000000000000, 0.000000000000000000, 1.000000000000000000 ) ) ;
#10755 = FACE_OUTER_BOUND ( 'NONE', #3536, .T. ) ;
#10756 = LINE ( 'NONE', #9840, #2063 ) ;
#10757 = CARTESIAN_POINT ( 'NONE',  ( -15.00000000000000000, 44.00000000000001421, 0.000000000000000000 ) ) ;
#10758 = ORIENTED_EDGE ( 'NONE', *, *, #10129, .F. ) ;
#10759 = CYLINDRICAL_SURFACE ( 'NONE', #8373, 40.00000000000000711 ) ;
#10760 = EDGE_CURVE ( 'NONE', #11493, #777, #6500, .T. ) ;
#10761 = DIRECTION ( 'NONE',  ( 0.000000000000000000, -0.3826834323650971648, 0.9238795325112837409 ) ) ;
#10762 = EDGE_CURVE ( 'NONE', #811, #1905, #5549, .T. ) ;
#10763 = CIRCLE ( 'NONE', #3773, 24.99999999999998579 ) ;
#10764 = VERTEX_POINT ( 'NONE', #3614 ) ;
#10765 = DIRECTION ( 'NONE',  ( 1.000000000000000000, -0.000000000000000000, -0.000000000000000000 ) ) ;
#10766 = AXIS2_PLACEMENT_3D ( 'NONE', #9128, #9261, #10241 ) ;
#10767 = ORIENTED_EDGE ( 'NONE', *, *, #4858, .F. ) ;
#10768 = DIRECTION ( 'NONE',  ( 1.000000000000000000, -0.000000000000000000, -0.000000000000000000 ) ) ;
#10769 = CIRCLE ( 'NONE', #11165, 9.600000000009600853 ) ;
#10770 = CARTESIAN_POINT ( 'NONE',  ( 46.00000000000000000, 1.456773409934505593E-31, -36.99999999999998579 ) ) ;
#10771 = DIRECTION ( 'NONE',  ( 0.000000000000000000, 0.000000000000000000, 1.000000000000000000 ) ) ;
#10772 = CIRCLE ( 'NONE', #4375, 20.24900000002024569 ) ;
#10773 = CYLINDRICAL_SURFACE ( 'NONE', #3844, 7.200000000007202416 ) ;
#10774 = DIRECTION ( 'NONE',  ( 0.000000000000000000, 1.000000000000000000, 0.000000000000000000 ) ) ;
#10775 = ORIENTED_EDGE ( 'NONE', *, *, #11721, .F. ) ;
#10776 = ORIENTED_EDGE ( 'NONE', *, *, #8533, .T. ) ;
#10777 = PLANE ( 'NONE',  #4266 ) ;
#10778 = ORIENTED_EDGE ( 'NONE', *, *, #7927, .T. ) ;
#10779 = AXIS2_PLACEMENT_3D ( 'NONE', #8058, #2222, #8115 ) ;
#10780 = CIRCLE ( 'NONE', #6592, 5.100000000000000533 ) ;
#10781 = FACE_OUTER_BOUND ( 'NONE', #5999, .T. ) ;
#10782 = ORIENTED_EDGE ( 'NONE', *, *, #9372, .T. ) ;
#10783 = DIRECTION ( 'NONE',  ( 0.000000000000000000, 0.000000000000000000, 1.000000000000000000 ) ) ;
#10784 = CARTESIAN_POINT ( 'NONE',  ( 4.999999999999999112, 14.14998813191269633, 1.676853263447936726 ) ) ;
#10785 = DIRECTION ( 'NONE',  ( 0.000000000000000000, 0.000000000000000000, 1.000000000000000000 ) ) ;
#10786 = CARTESIAN_POINT ( 'NONE',  ( 33.00000000000000000, 7.960204194457796463E-16, -6.500000000000000888 ) ) ;
#10787 = VERTEX_POINT ( 'NONE', #4297 ) ;
#10788 = AXIS2_PLACEMENT_3D ( 'NONE', #6319, #4440, #8268 ) ;
#10789 = AXIS2_PLACEMENT_3D ( 'NONE', #7448, #12055, #870 ) ;
#10790 = ORIENTED_EDGE ( 'NONE', *, *, #10574, .T. ) ;
#10791 = FILL_AREA_STYLE ('',( #4112 ) ) ;
#10792 = VERTEX_POINT ( 'NONE', #7188 ) ;
#10793 = LINE ( 'NONE', #4114, #4825 ) ;
#10794 = CARTESIAN_POINT ( 'NONE',  ( 36.00000000000000711, 6.123233995736773185E-16, -46.99999999999999289 ) ) ;
#10795 = VECTOR ( 'NONE', #193, 1000.000000000000000 ) ;
#10796 = CIRCLE ( 'NONE', #8613, 5.000000000000004441 ) ;
#10797 = AXIS2_PLACEMENT_3D ( 'NONE', #9312, #4421, #1730 ) ;
#10798 = DIRECTION ( 'NONE',  ( 1.000000000000000000, 0.000000000000000000, 0.000000000000000000 ) ) ;
#10799 = EDGE_CURVE ( 'NONE', #8654, #5793, #8260, .T. ) ;
#10800 = EDGE_CURVE ( 'NONE', #4621, #11283, #5975, .T. ) ;
#10801 = ORIENTED_EDGE ( 'NONE', *, *, #10154, .F. ) ;
#10802 = DIRECTION ( 'NONE',  ( 1.000000000000000000, 0.000000000000000000, -0.000000000000000000 ) ) ;
#10803 = DIRECTION ( 'NONE',  ( 1.000000000000000000, 0.000000000000000000, 0.000000000000000000 ) ) ;
#10804 = CIRCLE ( 'NONE', #4019, 14.24900000001425227 ) ;
#10805 = ORIENTED_EDGE ( 'NONE', *, *, #6937, .F. ) ;
#10806 = AXIS2_PLACEMENT_3D ( 'NONE', #2758, #12075, #6585 ) ;
#10807 = DIRECTION ( 'NONE',  ( 1.000000000000000000, 0.000000000000000000, 0.000000000000000000 ) ) ;
#10808 = APPLICATION_PROTOCOL_DEFINITION ( 'draft international standard', 'automotive_design', 1998, #11752 ) ;
#10809 = AXIS2_PLACEMENT_3D ( 'NONE', #10664, #2094, #11518 ) ;
#10810 = CARTESIAN_POINT ( 'NONE',  ( 5.000000000000004441, 0.000000000000000000, 4.250000000000000000 ) ) ;
#10811 = AXIS2_PLACEMENT_3D ( 'NONE', #11852, #9069, #9123 ) ;
#10812 = FACE_OUTER_BOUND ( 'NONE', #2603, .T. ) ;
#10813 = ORIENTED_EDGE ( 'NONE', *, *, #10007, .T. ) ;
#10814 = DIRECTION ( 'NONE',  ( 1.000000000000000000, 0.000000000000000000, 0.000000000000000000 ) ) ;
#10815 = STYLED_ITEM ( 'NONE', ( #1162 ), #2564 ) ;
#10816 = VECTOR ( 'NONE', #6672, 1000.000000000000000 ) ;
#10817 = CIRCLE ( 'NONE', #1638, 21.00000000002100009 ) ;
#10818 = PRODUCT_DEFINITION_SHAPE ( 'NONE', 'NONE',  #3130 ) ;
#10819 = SURFACE_STYLE_FILL_AREA ( #4363 ) ;
#10820 = AXIS2_PLACEMENT_3D ( 'NONE', #6915, #3158, #10715 ) ;
#10821 = AXIS2_PLACEMENT_3D ( 'NONE', #11313, #2892, #3892 ) ;
#10822 = DIRECTION ( 'NONE',  ( 0.000000000000000000, -1.000000000000000000, 0.000000000000000000 ) ) ;
#10823 = DIRECTION ( 'NONE',  ( 0.1305261922200524616, -0.9914448613738103822, 0.000000000000000000 ) ) ;
#10824 = EDGE_CURVE ( 'NONE', #3785, #9031, #1990, .T. ) ;
#10825 = EDGE_CURVE ( 'NONE', #9277, #10072, #10357, .T. ) ;
#10826 = DIRECTION ( 'NONE',  ( -1.000000000000000000, -0.000000000000000000, 0.000000000000000000 ) ) ;
#10827 = CARTESIAN_POINT ( 'NONE',  ( 0.000000000000000000, 15.37949036966230132, -13.17168466712912434 ) ) ;
#10828 = EDGE_CURVE ( 'NONE', #3326, #4782, #8374, .T. ) ;
#10829 = VERTEX_POINT ( 'NONE', #3802 ) ;
#10830 = EDGE_LOOP ( 'NONE', ( #10612, #6520 ) ) ;
#10831 = FACE_OUTER_BOUND ( 'NONE', #2503, .T. ) ;
#10832 = CARTESIAN_POINT ( 'NONE',  ( 36.00000000000000000, 40.00000000000000711, -19.99999999999998934 ) ) ;
#10833 = AXIS2_PLACEMENT_3D ( 'NONE', #10896, #6146, #8914 ) ;
#10834 = ORIENTED_EDGE ( 'NONE', *, *, #807, .T. ) ;
#10835 = PLANE ( 'NONE',  #6092 ) ;
#10836 = VECTOR ( 'NONE', #68, 1000.000000000000000 ) ;
#10837 = ORIENTED_EDGE ( 'NONE', *, *, #10968, .F. ) ;
#10838 = DIRECTION ( 'NONE',  ( 1.000000000000000000, -0.000000000000000000, -0.000000000000000000 ) ) ;
#10839 = ADVANCED_FACE ( 'NONE', ( #8686, #110 ), #981, .T. ) ;
#10840 = PRODUCT_DEFINITION_FORMATION_WITH_SPECIFIED_SOURCE ( 'ANY', '', #10302, .NOT_KNOWN. ) ;
#10841 = AXIS2_PLACEMENT_3D ( 'NONE', #7328, #7273, #7508 ) ;
#10842 = PRESENTATION_LAYER_ASSIGNMENT (  '', '', ( #7661 ) ) ;
#10843 =( NAMED_UNIT ( * ) PLANE_ANGLE_UNIT ( ) SI_UNIT ( $, .RADIAN. ) );
#10844 = CARTESIAN_POINT ( 'NONE',  ( 46.00000000000000000, 3.500000000000001332, -38.49999999999998579 ) ) ;
#10845 = AXIS2_PLACEMENT_3D ( 'NONE', #1506, #4442, #3630 ) ;
#10846 = CARTESIAN_POINT ( 'NONE',  ( 0.000000000000000000, 6.799999999999999822, 0.000000000000000000 ) ) ;
#10847 = CARTESIAN_POINT ( 'NONE',  ( 45.00000000000000000, 0.000000000000000000, 5.000000000000000000 ) ) ;
#10848 = ORIENTED_EDGE ( 'NONE', *, *, #11124, .F. ) ;
#10849 = ORIENTED_EDGE ( 'NONE', *, *, #9079, .F. ) ;
#10850 = DIRECTION ( 'NONE',  ( -1.000000000000000000, -3.903127820947815962E-18, 0.000000000000000000 ) ) ;
#10851 = ORIENTED_EDGE ( 'NONE', *, *, #1051, .F. ) ;
#10852 = AXIS2_PLACEMENT_3D ( 'NONE', #12302, #6646, #10443 ) ;
#10853 = EDGE_CURVE ( 'NONE', #3834, #12241, #10566, .T. ) ;
#10854 = DIRECTION ( 'NONE',  ( -1.000000000000000000, 0.000000000000000000, -0.000000000000000000 ) ) ;
#10855 = DIRECTION ( 'NONE',  ( 0.000000000000000000, 0.000000000000000000, -1.000000000000000000 ) ) ;
#10856 = DIRECTION ( 'NONE',  ( 0.000000000000000000, 0.000000000000000000, -1.000000000000000000 ) ) ;
#10857 = DIRECTION ( 'NONE',  ( -1.000000000000000000, -0.000000000000000000, -0.000000000000000000 ) ) ;
#10858 = CARTESIAN_POINT ( 'NONE',  ( 0.000000000000000000, 0.000000000000000000, 0.000000000000000000 ) ) ;
#10859 = VERTEX_POINT ( 'NONE', #2732 ) ;
#10860 = CARTESIAN_POINT ( 'NONE',  ( -13.05124837953327344, 0.000000000000000000, -41.99999999999999289 ) ) ;
#10861 = ORIENTED_EDGE ( 'NONE', *, *, #5770, .F. ) ;
#10862 =( LENGTH_UNIT ( ) NAMED_UNIT ( * ) SI_UNIT ( .MILLI., .METRE. ) );
#10863 = ORIENTED_EDGE ( 'NONE', *, *, #2583, .F. ) ;
#10864 = DIRECTION ( 'NONE',  ( 0.000000000000000000, 0.000000000000000000, 1.000000000000000000 ) ) ;
#10865 = CARTESIAN_POINT ( 'NONE',  ( 0.000000000000000000, 22.37914155802285876, -2.791921004064323864 ) ) ;
#10866 =( GEOMETRIC_REPRESENTATION_CONTEXT ( 3 ) GLOBAL_UNCERTAINTY_ASSIGNED_CONTEXT ( ( #11144 ) ) GLOBAL_UNIT_ASSIGNED_CONTEXT ( ( #2395, #9160, #12019 ) ) REPRESENTATION_CONTEXT ( 'NONE', 'WORKASPACE' ) );
#10867 = CYLINDRICAL_SURFACE ( 'NONE', #6008, 9.600000000009600853 ) ;
#10868 = VERTEX_POINT ( 'NONE', #12290 ) ;
#10869 = DIRECTION ( 'NONE',  ( 0.000000000000000000, 0.000000000000000000, 1.000000000000000000 ) ) ;
#10870 = ORIENTED_EDGE ( 'NONE', *, *, #7144, .F. ) ;
#10871 = CARTESIAN_POINT ( 'NONE',  ( 0.000000000000000000, 22.05152472667151642, -15.57980286237449619 ) ) ;
#10872 = CIRCLE ( 'NONE', #8692, 12.49999999999999645 ) ;
#10873 =( NAMED_UNIT ( * ) PLANE_ANGLE_UNIT ( ) SI_UNIT ( $, .RADIAN. ) );
#10874 = CARTESIAN_POINT ( 'NONE',  ( 4.999999999999999112, 1.676853263447885878, 14.14998813191270166 ) ) ;
#10875 = FACE_OUTER_BOUND ( 'NONE', #6907, .T. ) ;
#10876 = EDGE_CURVE ( 'NONE', #6875, #4331, #4970, .T. ) ;
#10877 = EDGE_LOOP ( 'NONE', ( #3615, #10902, #11920, #7523 ) ) ;
#10878 = CARTESIAN_POINT ( 'NONE',  ( 24.00000000000000000, 0.000000000000000000, -41.99999999999999289 ) ) ;
#10879 = EDGE_CURVE ( 'NONE', #231, #4639, #188, .T. ) ;
#10880 = DIRECTION ( 'NONE',  ( 0.000000000000000000, 0.000000000000000000, -1.000000000000000000 ) ) ;
#10881 = LINE ( 'NONE', #4130, #3216 ) ;
#10882 = CARTESIAN_POINT ( 'NONE',  ( 29.56763832957518545, 6.799999999999998046, 0.000000000000000000 ) ) ;
#10883 = CARTESIAN_POINT ( 'NONE',  ( 46.00000000000000000, 1.456773409934505593E-31, -41.99999999999998579 ) ) ;
#10884 = ORIENTED_EDGE ( 'NONE', *, *, #3715, .F. ) ;
#10885 = VERTEX_POINT ( 'NONE', #4799 ) ;
#10886 = CARTESIAN_POINT ( 'NONE',  ( 76.00000000000000000, 46.00000000000001421, -46.00000000000000000 ) ) ;
#10887 = CARTESIAN_POINT ( 'NONE',  ( 36.00000000000000711, 0.000000000000000000, 6.500000000000000888 ) ) ;
#10888 = ORIENTED_EDGE ( 'NONE', *, *, #4335, .T. ) ;
#10889 = CARTESIAN_POINT ( 'NONE',  ( 37.00000000000000711, -4.104405154062230115E-16, -2.224720805914714718E-17 ) ) ;
#10890 = EDGE_CURVE ( 'NONE', #9966, #7407, #10355, .T. ) ;
#10891 = ORIENTED_EDGE ( 'NONE', *, *, #7267, .T. ) ;
#10892 = DIRECTION ( 'NONE',  ( -0.000000000000000000, 0.000000000000000000, 1.000000000000000000 ) ) ;
#10893 = EDGE_CURVE ( 'NONE', #5929, #9771, #11554, .T. ) ;
#10894 = EDGE_CURVE ( 'NONE', #10885, #11449, #1933, .T. ) ;
#10895 = DIRECTION ( 'NONE',  ( 0.000000000000000000, 0.000000000000000000, -1.000000000000000000 ) ) ;
#10896 = CARTESIAN_POINT ( 'NONE',  ( 15.00000000000000355, 40.00000000000000711, 0.000000000000000000 ) ) ;
#10897 = LINE ( 'NONE', #6147, #10415 ) ;
#10898 = ORIENTED_EDGE ( 'NONE', *, *, #8151, .F. ) ;
#10899 = DIRECTION ( 'NONE',  ( 0.000000000000000000, -1.000000000000000000, 0.000000000000000000 ) ) ;
#10900 = ORIENTED_EDGE ( 'NONE', *, *, #9376, .T. ) ;
#10901 = FILL_AREA_STYLE ('',( #5034 ) ) ;
#10902 = ORIENTED_EDGE ( 'NONE', *, *, #4148, .T. ) ;
#10903 = PRODUCT_RELATED_PRODUCT_CATEGORY ( 'part', '', ( #6516 ) ) ;
#10904 = CARTESIAN_POINT ( 'NONE',  ( 0.000000000000000000, 7.654042494670957606E-16, -6.250000000000000000 ) ) ;
#10905 = CARTESIAN_POINT ( 'NONE',  ( 4.999999999999999112, 21.74405275335758247, 5.984728032765037398 ) ) ;
#10906 = FACE_OUTER_BOUND ( 'NONE', #7921, .T. ) ;
#10907 = DIRECTION ( 'NONE',  ( 0.000000000000000000, 0.000000000000000000, 1.000000000000000000 ) ) ;
#10908 = LINE ( 'NONE', #9802, #9213 ) ;
#10909 = EDGE_LOOP ( 'NONE', ( #5210, #4651, #12200, #11483 ) ) ;
#10910 = CARTESIAN_POINT ( 'NONE',  ( -20.00000000000000000, 3.061616997868383043E-15, -25.00000000000000000 ) ) ;
#10911 = ORIENTED_EDGE ( 'NONE', *, *, #9636, .T. ) ;
#10912 = ADVANCED_FACE ( 'NONE', ( #8558 ), #4613, .T. ) ;
#10914 = EDGE_CURVE ( 'NONE', #1609, #3733, #3370, .T. ) ;
#10913 = VERTEX_POINT ( 'NONE', #11350 ) ;
#10915 = DIRECTION ( 'NONE',  ( -1.000000000000000000, 0.000000000000000000, 0.000000000000000000 ) ) ;
#10916 = PRODUCT_DEFINITION_SHAPE ( 'NONE', 'NONE',  #12363 ) ;
#10917 = CARTESIAN_POINT ( 'NONE',  ( -10.00000000000000000, 0.000000000000000000, 0.000000000000000000 ) ) ;
#10918 = ADVANCED_BREP_SHAPE_REPRESENTATION ( '', ( #4645, #6056 ), #10046 ) ;
#10919 = VERTEX_POINT ( 'NONE', #9554 ) ;
#10920 = DIRECTION ( 'NONE',  ( -1.000000000000000000, -0.000000000000000000, 0.000000000000000000 ) ) ;
#10921 = ORIENTED_EDGE ( 'NONE', *, *, #9313, .F. ) ;
#10922 = LINE ( 'NONE', #2121, #10554 ) ;
#10923 = ORIENTED_EDGE ( 'NONE', *, *, #2717, .T. ) ;
#10924 = DIRECTION ( 'NONE',  ( -1.000000000000000000, -0.000000000000000000, 0.000000000000000000 ) ) ;
#10925 = DIRECTION ( 'NONE',  ( -1.000000000000000000, -0.000000000000000000, 0.000000000000000000 ) ) ;
#10926 = ORIENTED_EDGE ( 'NONE', *, *, #8072, .F. ) ;
#10927 = LINE ( 'NONE', #3319, #9984 ) ;
#10928 = CYLINDRICAL_SURFACE ( 'NONE', #596, 7.500000000000000888 ) ;
#10929 = DIRECTION ( 'NONE',  ( 0.000000000000000000, -1.000000000000000000, 0.000000000000000000 ) ) ;
#10930 = FACE_OUTER_BOUND ( 'NONE', #8733, .T. ) ;
#10931 = DIRECTION ( 'NONE',  ( 0.000000000000000000, 0.000000000000000000, -1.000000000000000000 ) ) ;
#10932 = DIRECTION ( 'NONE',  ( -1.000000000000000000, -0.000000000000000000, -0.000000000000000000 ) ) ;
#10933 = ORIENTED_EDGE ( 'NONE', *, *, #2399, .F. ) ;
#10934 = VERTEX_POINT ( 'NONE', #3683 ) ;
#10935 = ADVANCED_FACE ( 'NONE', ( #4681 ), #50, .T. ) ;
#10936 = CARTESIAN_POINT ( 'NONE',  ( 0.000000000000000000, 19.24938187143295920, 6.283573709965377674 ) ) ;
#10937 = FILL_AREA_STYLE ('',( #11997 ) ) ;
#10938 = DIRECTION ( 'NONE',  ( -1.000000000000000000, -0.000000000000000000, -0.000000000000000000 ) ) ;
#10939 = ORIENTED_EDGE ( 'NONE', *, *, #12053, .T. ) ;
#10940 = DIRECTION ( 'NONE',  ( 1.000000000000000000, 0.000000000000000000, 0.000000000000000000 ) ) ;
#10941 = ORIENTED_EDGE ( 'NONE', *, *, #3660, .F. ) ;
#10942 = CYLINDRICAL_SURFACE ( 'NONE', #9633, 6.500000000000000888 ) ;
#10943 = AXIS2_PLACEMENT_3D ( 'NONE', #2115, #5936, #7883 ) ;
#10944 = AXIS2_PLACEMENT_3D ( 'NONE', #8153, #637, #11018 ) ;
#10945 = DIRECTION ( 'NONE',  ( -0.000000000000000000, 1.000000000000000000, -0.000000000000000000 ) ) ;
#10946 = EDGE_CURVE ( 'NONE', #2532, #2177, #7691, .T. ) ;
#10947 = CYLINDRICAL_SURFACE ( 'NONE', #11227, 9.600000000009602630 ) ;
#10948 = CARTESIAN_POINT ( 'NONE',  ( 0.000000000000000000, -5.955107813822308138, -26.33508479058327367 ) ) ;
#10949 = AXIS2_PLACEMENT_3D ( 'NONE', #8218, #1707, #5338 ) ;
#10950 =( REPRESENTATION_RELATIONSHIP ('NONE','NONE', #9709, #10563 ) REPRESENTATION_RELATIONSHIP_WITH_TRANSFORMATION ( #11768 )SHAPE_REPRESENTATION_RELATIONSHIP( ) );
#10951 = AXIS2_PLACEMENT_3D ( 'NONE', #9003, #1176, #7999 ) ;
#10952 = ORIENTED_EDGE ( 'NONE', *, *, #6389, .F. ) ;
#10953 = EDGE_CURVE ( 'NONE', #6970, #7624, #5576, .T. ) ;
#10954 = FACE_OUTER_BOUND ( 'NONE', #9189, .T. ) ;
#10955 = LINE ( 'NONE', #3061, #6627 ) ;
#10956 = EDGE_CURVE ( 'NONE', #9537, #6756, #12350, .T. ) ;
#10957 = ORIENTED_EDGE ( 'NONE', *, *, #6033, .F. ) ;
#10958 = ORIENTED_EDGE ( 'NONE', *, *, #8770, .T. ) ;
#10959 = AXIS2_PLACEMENT_3D ( 'NONE', #7525, #2757, #4895 ) ;
#10960 = AXIS2_PLACEMENT_3D ( 'NONE', #12347, #3870, #2795 ) ;
#10961 = DIRECTION ( 'NONE',  ( 0.000000000000000000, 0.000000000000000000, 1.000000000000000000 ) ) ;
#10962 = CLOSED_SHELL ( 'NONE', ( #11928, #2020, #3284, #6622, #8442, #638, #8918, #4319, #6720, #951, #8556, #4546, #9373, #1963, #8870, #6458, #565, #9030, #2496, #3958, #11052, #2067, #287, #9220, #7035, #5527, #5083, #9314 ) ) ;
#10963 = LINE ( 'NONE', #2338, #7395 ) ;
#10964 = CARTESIAN_POINT ( 'NONE',  ( 46.00000000000000000, 1.444447458290426890E-31, -41.99999999999998579 ) ) ;
#10965 = DIRECTION ( 'NONE',  ( -1.000000000000000000, 0.000000000000000000, 0.000000000000000000 ) ) ;
#10966 = CARTESIAN_POINT ( 'NONE',  ( -20.63749999999999574, 0.000000000000000000, 0.000000000000000000 ) ) ;
#10967 = ORIENTED_EDGE ( 'NONE', *, *, #5785, .T. ) ;
#10968 = EDGE_CURVE ( 'NONE', #4264, #8081, #1578, .T. ) ;
#10969 = ADVANCED_FACE ( 'NONE', ( #4868 ), #3926, .T. ) ;
#10970 = CARTESIAN_POINT ( 'NONE',  ( 4.999999999999999112, 5.984728032764962791, 21.74405275335760379 ) ) ;
#10971 = EDGE_CURVE ( 'NONE', #4639, #231, #10166, .T. ) ;
#10972 = AXIS2_PLACEMENT_3D ( 'NONE', #1983, #1045, #11593 ) ;
#10973 = ORIENTED_EDGE ( 'NONE', *, *, #9103, .T. ) ;
#10974 = DIRECTION ( 'NONE',  ( -1.000000000000000000, -3.903127820947815962E-18, 0.000000000000000000 ) ) ;
#10975 = VERTEX_POINT ( 'NONE', #11944 ) ;
#10976 = VECTOR ( 'NONE', #10366, 1000.000000000000000 ) ;
#10977 = DIRECTION ( 'NONE',  ( 0.000000000000000000, 0.000000000000000000, -1.000000000000000000 ) ) ;
#10978 = DIRECTION ( 'NONE',  ( 0.000000000000000000, 0.000000000000000000, -1.000000000000000000 ) ) ;
#10979 = VERTEX_POINT ( 'NONE', #9158 ) ;
#10980 = PLANE ( 'NONE',  #2204 ) ;
#10981 = EDGE_CURVE ( 'NONE', #5342, #1003, #9913, .T. ) ;
#10982 = EDGE_CURVE ( 'NONE', #3672, #7335, #6370, .T. ) ;
#10983 = AXIS2_PLACEMENT_3D ( 'NONE', #3071, #11435, #8565 ) ;
#10984 = ORIENTED_EDGE ( 'NONE', *, *, #11833, .T. ) ;
#10985 = CARTESIAN_POINT ( 'NONE',  ( 2.500000000000000000, 2.357898499370433054, -1.951563910473907981E-15 ) ) ;
#10986 = ORIENTED_EDGE ( 'NONE', *, *, #8783, .T. ) ;
#10987 = PRESENTATION_STYLE_ASSIGNMENT (( #4429 ) ) ;
#10988 = VECTOR ( 'NONE', #9016, 1000.000000000000000 ) ;
#10989 = CARTESIAN_POINT ( 'NONE',  ( 4.999999999999999112, -17.79862902732255137, -13.85025647830076245 ) ) ;
#10990 = VECTOR ( 'NONE', #859, 1000.000000000000000 ) ;
#10991 = ORIENTED_EDGE ( 'NONE', *, *, #1399, .F. ) ;
#10992 = FACE_OUTER_BOUND ( 'NONE', #5682, .T. ) ;
#10993 = CIRCLE ( 'NONE', #8615, 21.00000000002100009 ) ;
#10994 = CARTESIAN_POINT ( 'NONE',  ( 42.00000000000000000, -2.941673623582830022, 4.043087470277766826 ) ) ;
#10995 = EDGE_CURVE ( 'NONE', #7542, #4122, #4330, .T. ) ;
#10996 = CIRCLE ( 'NONE', #5018, 27.00000000002699707 ) ;
#10997 = CIRCLE ( 'NONE', #1622, 7.000000000000006217 ) ;
#10998 = CARTESIAN_POINT ( 'NONE',  ( 46.00000000000000000, 1.456773409934505593E-31, -41.99999999999998579 ) ) ;
#10999 = CARTESIAN_POINT ( 'NONE',  ( 0.000000000000000000, 6.799999999999999822, -1.500000000000000000 ) ) ;
#11000 = AXIS2_PLACEMENT_3D ( 'NONE', #7441, #4617, #3685 ) ;
#11001 = DIRECTION ( 'NONE',  ( 1.000000000000000000, 0.000000000000000000, 0.000000000000000000 ) ) ;
#11002 = LINE ( 'NONE', #11068, #5651 ) ;
#11003 = VERTEX_POINT ( 'NONE', #7102 ) ;
#11004 = VERTEX_POINT ( 'NONE', #1331 ) ;
#11005 = CARTESIAN_POINT ( 'NONE',  ( 0.000000000000000000, 0.000000000000000000, 0.000000000000000000 ) ) ;
#11006 = CARTESIAN_POINT ( 'NONE',  ( 43.00000000000000000, -2.824006678639516377, 3.881363971466655904 ) ) ;
#11007 = VERTEX_POINT ( 'NONE', #6286 ) ;
#11008 = CYLINDRICAL_SURFACE ( 'NONE', #4093, 25.00000000000000000 ) ;
#11009 = EDGE_LOOP ( 'NONE', ( #4343, #7091 ) ) ;
#11010 = PLANE ( 'NONE',  #2428 ) ;
#11011 = STYLED_ITEM ( 'NONE', ( #11924 ), #4209 ) ;
#11012 = CIRCLE ( 'NONE', #9638, 27.00000000002699707 ) ;
#11013 = AXIS2_PLACEMENT_3D ( 'NONE', #2006, #11369, #11440 ) ;
#11014 = AXIS2_PLACEMENT_3D ( 'NONE', #8667, #9670, #150 ) ;
#11015 = AXIS2_PLACEMENT_3D ( 'NONE', #1698, #11188, #8149 ) ;
#11016 = VERTEX_POINT ( 'NONE', #9965 ) ;
#11017 = CYLINDRICAL_SURFACE ( 'NONE', #1416, 4.250000000000000000 ) ;
#11018 = DIRECTION ( 'NONE',  ( 0.000000000000000000, 0.9238795325112878487, -0.3826834323650872283 ) ) ;
#11019 = CARTESIAN_POINT ( 'NONE',  ( 0.000000000000000000, 14.14998813191269633, 1.676853263447936726 ) ) ;
#11020 = CARTESIAN_POINT ( 'NONE',  ( -36.00000000000000711, 0.000000000000000000, 0.000000000000000000 ) ) ;
#11021 = AXIS2_PLACEMENT_3D ( 'NONE', #6521, #10320, #1759 ) ;
#11022 = CIRCLE ( 'NONE', #2642, 7.500000000000000888 ) ;
#11023 = ORIENTED_EDGE ( 'NONE', *, *, #12093, .F. ) ;
#11024 = LINE ( 'NONE', #2461, #12134 ) ;
#11025 = VECTOR ( 'NONE', #10265, 1000.000000000000000 ) ;
#11026 = CARTESIAN_POINT ( 'NONE',  ( 37.00000000000000711, 6.799999999999998046, 0.000000000000000000 ) ) ;
#11027 = VERTEX_POINT ( 'NONE', #391 ) ;
#11028 = CARTESIAN_POINT ( 'NONE',  ( 2.499999999999999556, 5.950465759859149273, -20.13931372320382351 ) ) ;
#11029 = ORIENTED_EDGE ( 'NONE', *, *, #5391, .T. ) ;
#11030 = EDGE_CURVE ( 'NONE', #5880, #11004, #1417, .T. ) ;
#11031 = AXIS2_PLACEMENT_3D ( 'NONE', #6488, #9306, #12279 ) ;
#11032 = CIRCLE ( 'NONE', #1846, 27.00000000002699707 ) ;
#11033 = VECTOR ( 'NONE', #7055, 1000.000000000000000 ) ;
#11034 = EDGE_CURVE ( 'NONE', #7184, #3862, #575, .T. ) ;
#11035 = AXIS2_PLACEMENT_3D ( 'NONE', #1135, #4132, #196 ) ;
#11036 = DIRECTION ( 'NONE',  ( 0.000000000000000000, 0.3826834323650905589, -0.9238795325112864054 ) ) ;
#11037 = DIRECTION ( 'NONE',  ( -1.000000000000000000, 0.000000000000000000, 0.000000000000000000 ) ) ;
#11038 = FACE_BOUND ( 'NONE', #6694, .T. ) ;
#11039 = CARTESIAN_POINT ( 'NONE',  ( 0.000000000000000000, -9.168210874537708222, 18.05452603534162748 ) ) ;
#11040 = DIRECTION ( 'NONE',  ( 0.000000000000000000, 0.000000000000000000, 1.000000000000000000 ) ) ;
#11041 = VERTEX_POINT ( 'NONE', #8049 ) ;
#11042 = CARTESIAN_POINT ( 'NONE',  ( -20.63749999999999574, 0.000000000000000000, 0.000000000000000000 ) ) ;
#11043 = ORIENTED_EDGE ( 'NONE', *, *, #11030, .T. ) ;
#11044 = DIRECTION ( 'NONE',  ( -1.000000000000000000, 0.000000000000000000, 0.000000000000000000 ) ) ;
#11045 = AXIS2_PLACEMENT_3D ( 'NONE', #2690, #743, #8453 ) ;
#11046 = ORIENTED_EDGE ( 'NONE', *, *, #4551, .T. ) ;
#11047 = DIRECTION ( 'NONE',  ( 1.000000000000000000, -0.000000000000000000, -0.000000000000000000 ) ) ;
#11048 = EDGE_CURVE ( 'NONE', #3603, #8107, #814, .T. ) ;
#11049 = DIRECTION ( 'NONE',  ( -1.000000000000000000, -0.000000000000000000, 0.000000000000000000 ) ) ;
#11050 = EDGE_CURVE ( 'NONE', #10239, #4391, #464, .T. ) ;
#11051 = EDGE_CURVE ( 'NONE', #3907, #1528, #11087, .T. ) ;
#11052 = ADVANCED_FACE ( 'NONE', ( #2330 ), #10681, .T. ) ;
#11053 = VERTEX_POINT ( 'NONE', #9109 ) ;
#11054 = DIRECTION ( 'NONE',  ( -1.000000000000000000, 0.000000000000000000, 0.000000000000000000 ) ) ;
#11055 =( GEOMETRIC_REPRESENTATION_CONTEXT ( 3 ) GLOBAL_UNCERTAINTY_ASSIGNED_CONTEXT ( ( #9527 ) ) GLOBAL_UNIT_ASSIGNED_CONTEXT ( ( #1597, #4411, #12036 ) ) REPRESENTATION_CONTEXT ( 'NONE', 'WORKASPACE' ) );
#11056 = ORIENTED_EDGE ( 'NONE', *, *, #4396, .F. ) ;
#11057 = CARTESIAN_POINT ( 'NONE',  ( 4.999999999999999112, -0.4834863907626938961, 16.90755573046746107 ) ) ;
#11058 = ORIENTED_EDGE ( 'NONE', *, *, #9531, .T. ) ;
#11059 = FACE_OUTER_BOUND ( 'NONE', #8717, .T. ) ;
#11060 = AXIS2_PLACEMENT_3D ( 'NONE', #8974, #8111, #3109 ) ;
#11061 = ORIENTED_EDGE ( 'NONE', *, *, #10006, .F. ) ;
#11062 = DIRECTION ( 'NONE',  ( 0.000000000000000000, 0.000000000000000000, -1.000000000000000000 ) ) ;
#11063 = CARTESIAN_POINT ( 'NONE',  ( 0.000000000000000000, 5.622796541391564595, 13.09267581720868989 ) ) ;
#11064 = CARTESIAN_POINT ( 'NONE',  ( 65.79898987322334847, 5.744562646538025952, -46.00000000000000000 ) ) ;
#11065 = DIRECTION ( 'NONE',  ( -1.000000000000000000, -0.000000000000000000, -0.000000000000000000 ) ) ;
#11066 = AXIS2_PLACEMENT_3D ( 'NONE', #10889, #9953, #1378 ) ;
#11067 = DIRECTION ( 'NONE',  ( -0.000000000000000000, -1.000000000000000000, -0.000000000000000000 ) ) ;
#11068 = CARTESIAN_POINT ( 'NONE',  ( 2.499999999999998668, -4.916402349214727074, 20.41639017900857667 ) ) ;
#11069 = VERTEX_POINT ( 'NONE', #5339 ) ;
#11070 = ORIENTED_EDGE ( 'NONE', *, *, #2739, .F. ) ;
#11071 = CARTESIAN_POINT ( 'NONE',  ( 26.00000000000000355, 0.000000000000000000, 40.00000000000000711 ) ) ;
#11072 = SURFACE_STYLE_USAGE ( .BOTH. , #9203 ) ;
#11073 = LINE ( 'NONE', #12063, #5828 ) ;
#11074 = EDGE_LOOP ( 'NONE', ( #3432, #3632 ) ) ;
#11075 = DIRECTION ( 'NONE',  ( -1.000000000000000000, -0.000000000000000000, -0.000000000000000000 ) ) ;
#11076 = ADVANCED_FACE ( 'NONE', ( #6150 ), #7154, .F. ) ;
#11077 = ORIENTED_EDGE ( 'NONE', *, *, #10069, .F. ) ;
#11078 = DIRECTION ( 'NONE',  ( 0.000000000000000000, -1.000000000000000000, 1.287488025362403787E-15 ) ) ;
#11079 = EDGE_CURVE ( 'NONE', #9068, #10934, #10955, .T. ) ;
#11080 = CARTESIAN_POINT ( 'NONE',  ( 37.00000000000000711, 0.000000000000000000, 0.000000000000000000 ) ) ;
#11081 = CYLINDRICAL_SURFACE ( 'NONE', #8094, 2.000000000000000000 ) ;
#11082 = CARTESIAN_POINT ( 'NONE',  ( 4.999999999999999112, -13.85025647830044271, -17.79862902732279650 ) ) ;
#11083 = LINE ( 'NONE', #3393, #2437 ) ;
#11084 = EDGE_LOOP ( 'NONE', ( #7971, #6097 ) ) ;
#11085 = FACE_OUTER_BOUND ( 'NONE', #10877, .T. ) ;
#11086 = AXIS2_PLACEMENT_3D ( 'NONE', #6440, #10244, #5501 ) ;
#11087 = LINE ( 'NONE', #3470, #2221 ) ;
#11088 = ORIENTED_EDGE ( 'NONE', *, *, #1174, .T. ) ;
#11089 = CARTESIAN_POINT ( 'NONE',  ( -4.799999999999999822, 5.878304635907294211E-16, -1.000000000000000000 ) ) ;
#11090 = ORIENTED_EDGE ( 'NONE', *, *, #10217, .T. ) ;
#11091 = CARTESIAN_POINT ( 'NONE',  ( -0.1920286436967153787, 0.000000000000000000, 0.000000000000000000 ) ) ;
#11092 = DIRECTION ( 'NONE',  ( -1.000000000000000000, 0.000000000000000000, -0.000000000000000000 ) ) ;
#11093 = CARTESIAN_POINT ( 'NONE',  ( 0.000000000000000000, -21.74405275335762155, 5.984728032764886407 ) ) ;
#11094 = DIRECTION ( 'NONE',  ( 0.000000000000000000, 0.000000000000000000, 1.000000000000000000 ) ) ;
#11095 = CARTESIAN_POINT ( 'NONE',  ( 4.999999999999999112, 0.000000000000000000, 0.000000000000000000 ) ) ;
#11096 = ORIENTED_EDGE ( 'NONE', *, *, #119, .T. ) ;
#11097 = CARTESIAN_POINT ( 'NONE',  ( 26.00000000000000355, 34.64101615137756340, -19.99999999999998934 ) ) ;
#11098 = ORIENTED_EDGE ( 'NONE', *, *, #2888, .T. ) ;
#11099 = DIRECTION ( 'NONE',  ( -1.000000000000000000, 0.000000000000000000, 0.000000000000000000 ) ) ;
#11100 = EDGE_CURVE ( 'NONE', #1890, #2097, #8219, .T. ) ;
#11101 = ORIENTED_EDGE ( 'NONE', *, *, #1190, .T. ) ;
#11102 = LINE ( 'NONE', #5301, #2825 ) ;
#11103 = CARTESIAN_POINT ( 'NONE',  ( 0.000000000000000000, 8.035066368449204077, 14.88411597386731877 ) ) ;
#11104 = ORIENTED_EDGE ( 'NONE', *, *, #4875, .T. ) ;
#11105 = DIRECTION ( 'NONE',  ( 0.000000000000000000, 0.000000000000000000, -1.000000000000000000 ) ) ;
#11106 = EDGE_CURVE ( 'NONE', #4934, #8107, #3343, .T. ) ;
#11107 = EDGE_LOOP ( 'NONE', ( #5420, #1088, #9071, #11206 ) ) ;
#11108 = CARTESIAN_POINT ( 'NONE',  ( -2.354826896168714434, -6.962563485461402024, -1.000000000000000000 ) ) ;
#11109 = ORIENTED_EDGE ( 'NONE', *, *, #3493, .T. ) ;
#11110 = ADVANCED_FACE ( 'NONE', ( #4390 ), #12017, .T. ) ;
#11111 =( NAMED_UNIT ( * ) SI_UNIT ( $, .STERADIAN. ) SOLID_ANGLE_UNIT ( ) );
#11112 = EDGE_CURVE ( 'NONE', #11003, #4243, #10010, .T. ) ;
#11113 = DIRECTION ( 'NONE',  ( 1.000000000000000000, 0.000000000000000000, 0.000000000000000000 ) ) ;
#11114 = ORIENTED_EDGE ( 'NONE', *, *, #6016, .F. ) ;
#11115 = CARTESIAN_POINT ( 'NONE',  ( 0.000000000000000000, 0.000000000000000000, 0.000000000000000000 ) ) ;
#11116 = APPLICATION_CONTEXT ( 'automotive_design' ) ;
#11117 = CARTESIAN_POINT ( 'NONE',  ( 36.00000000000000711, 0.000000000000000000, 0.000000000000000000 ) ) ;
#11118 = DIRECTION ( 'NONE',  ( -1.000000000000000000, 0.000000000000000000, 0.000000000000000000 ) ) ;
#11119 = LINE ( 'NONE', #5447, #971 ) ;
#11120 = DIRECTION ( 'NONE',  ( 1.000000000000000000, 0.000000000000000000, 0.000000000000000000 ) ) ;
#11121 = ORIENTED_EDGE ( 'NONE', *, *, #9258, .T. ) ;
#11122 = VERTEX_POINT ( 'NONE', #9222 ) ;
#11123 = CARTESIAN_POINT ( 'NONE',  ( -19.99999999999999645, 0.000000000000000000, 0.000000000000000000 ) ) ;
#11124 = EDGE_CURVE ( 'NONE', #1740, #4492, #8472, .T. ) ;
#11125 = SURFACE_STYLE_USAGE ( .BOTH. , #3453 ) ;
#11126 = DIRECTION ( 'NONE',  ( 1.000000000000000000, 0.000000000000000000, 0.000000000000000000 ) ) ;
#11127 = ADVANCED_FACE ( 'NONE', ( #648 ), #6525, .T. ) ;
#11128 = ORIENTED_EDGE ( 'NONE', *, *, #10346, .T. ) ;
#11129 = FACE_BOUND ( 'NONE', #467, .T. ) ;
#11130 = ORIENTED_EDGE ( 'NONE', *, *, #11555, .F. ) ;
#11131 = LINE ( 'NONE', #10195, #7432 ) ;
#11132 = DIRECTION ( 'NONE',  ( 0.000000000000000000, 0.000000000000000000, 1.000000000000000000 ) ) ;
#11133 = LINE ( 'NONE', #8280, #11933 ) ;
#11134 = EDGE_CURVE ( 'NONE', #11902, #8475, #3828, .T. ) ;
#11135 = ADVANCED_FACE ( 'NONE', ( #1652, #10390 ), #4707, .F. ) ;
#11136 = DIRECTION ( 'NONE',  ( 0.000000000000000000, 0.000000000000000000, 1.000000000000000000 ) ) ;
#11137 = FACE_OUTER_BOUND ( 'NONE', #311, .T. ) ;
#11138 = EDGE_LOOP ( 'NONE', ( #6355, #1758, #57, #10891 ) ) ;
#11139 = CYLINDRICAL_SURFACE ( 'NONE', #9573, 7.200000000007202416 ) ;
#11140 = DIRECTION ( 'NONE',  ( 0.000000000000000000, -1.000000000000000000, 0.000000000000000000 ) ) ;
#11141 = AXIS2_PLACEMENT_3D ( 'NONE', #9711, #2130, #5948 ) ;
#11142 = ORIENTED_EDGE ( 'NONE', *, *, #1783, .T. ) ;
#11143 = DIRECTION ( 'NONE',  ( 0.000000000000000000, -1.000000000000000000, -1.036015409262890124E-14 ) ) ;
#11144 = UNCERTAINTY_MEASURE_WITH_UNIT (LENGTH_MEASURE( 1.000000000000000082E-05 ), #2395, 'distance_accuracy_value', 'NONE');
#11145 = EDGE_LOOP ( 'NONE', ( #11659, #2676 ) ) ;
#11146 = CIRCLE ( 'NONE', #962, 4.799999999999999822 ) ;
#11147 = LINE ( 'NONE', #6478, #8376 ) ;
#11148 = VECTOR ( 'NONE', #4234, 1000.000000000000000 ) ;
#11149 = FACE_OUTER_BOUND ( 'NONE', #8840, .T. ) ;
#11150 = DIRECTION ( 'NONE',  ( 0.000000000000000000, 0.3826834323650841752, 0.9238795325112890700 ) ) ;
#11151 = CIRCLE ( 'NONE', #8366, 2.396904916527700102 ) ;
#11152 = FACE_OUTER_BOUND ( 'NONE', #5653, .T. ) ;
#11153 = DIRECTION ( 'NONE',  ( -1.000000000000000000, 0.000000000000000000, -0.000000000000000000 ) ) ;
#11154 = EDGE_LOOP ( 'NONE', ( #3153, #9881, #4180, #9583 ) ) ;
#11155 = DIRECTION ( 'NONE',  ( 1.000000000000000000, 0.000000000000000000, 0.000000000000000000 ) ) ;
#11156 = ORIENTED_EDGE ( 'NONE', *, *, #9530, .T. ) ;
#11157 = CARTESIAN_POINT ( 'NONE',  ( 24.00000000000000000, 0.000000000000000000, -41.99999999999999289 ) ) ;
#11158 = PRODUCT_CONTEXT ( 'NONE', #11116, 'mechanical' ) ;
#11159 = ORIENTED_EDGE ( 'NONE', *, *, #3640, .F. ) ;
#11160 = PLANE ( 'NONE',  #2028 ) ;
#11161 = FACE_OUTER_BOUND ( 'NONE', #3742, .T. ) ;
#11162 = VECTOR ( 'NONE', #6047, 1000.000000000000000 ) ;
#11163 = ORIENTED_EDGE ( 'NONE', *, *, #4376, .F. ) ;
#11164 = DIRECTION ( 'NONE',  ( 1.000000000000000000, 0.000000000000000000, 0.000000000000000000 ) ) ;
#11165 = AXIS2_PLACEMENT_3D ( 'NONE', #5761, #9585, #8525 ) ;
#11166 = VECTOR ( 'NONE', #3007, 1000.000000000000000 ) ;
#11167 = ORIENTED_EDGE ( 'NONE', *, *, #8770, .F. ) ;
#11168 = CARTESIAN_POINT ( 'NONE',  ( 45.00000000000000000, 0.000000000000000000, 5.000000000000000000 ) ) ;
#11169 = ORIENTED_EDGE ( 'NONE', *, *, #10735, .F. ) ;
#11170 = FACE_OUTER_BOUND ( 'NONE', #4962, .T. ) ;
#11171 = EDGE_LOOP ( 'NONE', ( #1703, #3556, #12346, #4144 ) ) ;
#11172 = LINE ( 'NONE', #1500, #10365 ) ;
#11173 = AXIS2_PLACEMENT_3D ( 'NONE', #2400, #3297, #11843 ) ;
#11174 = EDGE_CURVE ( 'NONE', #4490, #9779, #7417, .T. ) ;
#11175 = AXIS2_PLACEMENT_3D ( 'NONE', #6700, #9750, #1170 ) ;
#11176 = CARTESIAN_POINT ( 'NONE',  ( 4.999999999999997335, 0.000000000000000000, 5.000000000000000000 ) ) ;
#11177 = EDGE_CURVE ( 'NONE', #7435, #10418, #6471, .T. ) ;
#11178 = DIRECTION ( 'NONE',  ( 1.000000000000000000, -0.000000000000000000, 0.000000000000000000 ) ) ;
#11179 = CARTESIAN_POINT ( 'NONE',  ( 1.600000000000000089, 0.000000000000000000, 0.000000000000000000 ) ) ;
#11180 = ORIENTED_EDGE ( 'NONE', *, *, #9102, .F. ) ;
#11181 = VERTEX_POINT ( 'NONE', #10269 ) ;
#11182 = DIRECTION ( 'NONE',  ( -1.000000000000000000, 0.000000000000000000, 0.000000000000000000 ) ) ;
#11183 = AXIS2_PLACEMENT_3D ( 'NONE', #6130, #1369, #2191 ) ;
#11184 = CYLINDRICAL_SURFACE ( 'NONE', #8634, 20.24900000002024569 ) ;
#11185 = AXIS2_PLACEMENT_3D ( 'NONE', #1543, #12043, #11164 ) ;
#11186 = DIRECTION ( 'NONE',  ( -1.734723475976807094E-16, 1.000000000000000000, 0.000000000000000000 ) ) ;
#11187 = ORIENTED_EDGE ( 'NONE', *, *, #2712, .F. ) ;
#11188 = DIRECTION ( 'NONE',  ( -1.000000000000000000, 0.000000000000000000, 0.000000000000000000 ) ) ;
#11189 = EDGE_CURVE ( 'NONE', #1430, #1455, #4618, .T. ) ;
#11190 = VECTOR ( 'NONE', #5072, 1000.000000000000000 ) ;
#11191 = AXIS2_PLACEMENT_3D ( 'NONE', #5146, #7222, #11601 ) ;
#11192 = EDGE_CURVE ( 'NONE', #12066, #103, #3712, .T. ) ;
#11193 = CIRCLE ( 'NONE', #10405, 25.00000000000000000 ) ;
#11194 = EDGE_CURVE ( 'NONE', #8297, #8639, #7629, .T. ) ;
#11195 = AXIS2_PLACEMENT_3D ( 'NONE', #1715, #6480, #9296 ) ;
#11196 = TOROIDAL_SURFACE ( 'NONE', #5823, 7.399999999999999467, 0.1000000000000000472 ) ;
#11197 = EDGE_CURVE ( 'NONE', #4830, #6538, #2617, .T. ) ;
#11198 = LINE ( 'NONE', #4513, #2397 ) ;
#11199 = LINE ( 'NONE', #7340, #4755 ) ;
#11200 = EDGE_LOOP ( 'NONE', ( #5719, #9522, #9484, #1885 ) ) ;
#11201 = CARTESIAN_POINT ( 'NONE',  ( 36.00000000000000000, 30.00000000000000711, 20.00000000000001066 ) ) ;
#11202 = CARTESIAN_POINT ( 'NONE',  ( 0.000000000000000000, 0.000000000000000000, 1.500000000000000000 ) ) ;
#11203 = ORIENTED_EDGE ( 'NONE', *, *, #1397, .F. ) ;
#11204 = CARTESIAN_POINT ( 'NONE',  ( 0.000000000000000000, 20.18872947935930995, 1.561154383803294410 ) ) ;
#11205 = DIRECTION ( 'NONE',  ( 0.000000000000000000, -1.000000000000000000, 0.000000000000000000 ) ) ;
#11206 = ORIENTED_EDGE ( 'NONE', *, *, #1804, .T. ) ;
#11207 = DIRECTION ( 'NONE',  ( 0.000000000000000000, 0.000000000000000000, 1.000000000000000000 ) ) ;
#11208 = CIRCLE ( 'NONE', #8231, 6.080745460913608902 ) ;
#11209 = VERTEX_POINT ( 'NONE', #5400 ) ;
#11210 = AXIS2_PLACEMENT_3D ( 'NONE', #4265, #9032, #323 ) ;
#11211 = EDGE_CURVE ( 'NONE', #5674, #7263, #7471, .T. ) ;
#11212 = DIRECTION ( 'NONE',  ( 0.000000000000000000, 0.000000000000000000, 1.000000000000000000 ) ) ;
#11213 = MECHANICAL_DESIGN_GEOMETRIC_PRESENTATION_REPRESENTATION (  '', ( #10815 ), #7651 ) ;
#11214 = AXIS2_PLACEMENT_3D ( 'NONE', #4155, #10965, #10907 ) ;
#11215 = CYLINDRICAL_SURFACE ( 'NONE', #1195, 9.600000000009600853 ) ;
#11216 = LINE ( 'NONE', #91, #7826 ) ;
#11217 = LINE ( 'NONE', #12323, #10627 ) ;
#11218 = DIRECTION ( 'NONE',  ( 0.000000000000000000, 0.000000000000000000, -1.000000000000000000 ) ) ;
#11219 = VERTEX_POINT ( 'NONE', #708 ) ;
#11220 = ORIENTED_EDGE ( 'NONE', *, *, #9355, .T. ) ;
#11221 = LINE ( 'NONE', #2663, #1221 ) ;
#11222 = ORIENTED_EDGE ( 'NONE', *, *, #4535, .F. ) ;
#11223 = CARTESIAN_POINT ( 'NONE',  ( 4.999999999999999112, -26.33508479058316354, -5.955107813822782425 ) ) ;
#11224 = SHAPE_DEFINITION_REPRESENTATION ( #4619, #5877 ) ;
#11225 = ORIENTED_EDGE ( 'NONE', *, *, #11406, .T. ) ;
#11226 = PRODUCT_DEFINITION_FORMATION_WITH_SPECIFIED_SOURCE ( 'ANY', '', #7730, .NOT_KNOWN. ) ;
#11227 = AXIS2_PLACEMENT_3D ( 'NONE', #6036, #4202, #11702 ) ;
#11228 = DIRECTION ( 'NONE',  ( -1.000000000000000000, 0.000000000000000000, 0.000000000000000000 ) ) ;
#11229 = VECTOR ( 'NONE', #5945, 1000.000000000000000 ) ;
#11230 = EDGE_CURVE ( 'NONE', #10148, #11485, #4020, .T. ) ;
#11231 = CIRCLE ( 'NONE', #1459, 27.00000000002699707 ) ;
#11232 = DIRECTION ( 'NONE',  ( 0.000000000000000000, 0.000000000000000000, 1.000000000000000000 ) ) ;
#11233 = EDGE_CURVE ( 'NONE', #3600, #6059, #2823, .T. ) ;
#11234 = ORIENTED_EDGE ( 'NONE', *, *, #7002, .T. ) ;
#11235 = LINE ( 'NONE', #12153, #7619 ) ;
#11236 = DIRECTION ( 'NONE',  ( 1.000000000000000000, 1.734723475976807094E-16, 0.000000000000000000 ) ) ;
#11237 = ORIENTED_EDGE ( 'NONE', *, *, #9515, .F. ) ;
#11238 = CIRCLE ( 'NONE', #5863, 1.999999999999998224 ) ;
#11239 = CARTESIAN_POINT ( 'NONE',  ( 15.00000000000000355, 44.00000000000001421, -2.149999999999999023 ) ) ;
#11240 = VERTEX_POINT ( 'NONE', #5522 ) ;
#11241 =( NAMED_UNIT ( * ) PLANE_ANGLE_UNIT ( ) SI_UNIT ( $, .RADIAN. ) );
#11242 = CARTESIAN_POINT ( 'NONE',  ( 0.000000000000000000, -4.576198416197066798, -26.60936692326695407 ) ) ;
#11243 = VERTEX_POINT ( 'NONE', #11385 ) ;
#11244 = DIRECTION ( 'NONE',  ( 0.000000000000000000, 0.000000000000000000, -1.000000000000000000 ) ) ;
#11245 = VECTOR ( 'NONE', #9568, 1000.000000000000000 ) ;
#11246 = DIRECTION ( 'NONE',  ( -1.000000000000000000, 0.000000000000000000, 0.000000000000000000 ) ) ;
#11247 = DIRECTION ( 'NONE',  ( 0.000000000000000000, 0.000000000000000000, 1.000000000000000000 ) ) ;
#11248 = DIRECTION ( 'NONE',  ( 0.000000000000000000, 1.000000000000000000, 3.491481338843133355E-15 ) ) ;
#11249 = ORIENTED_EDGE ( 'NONE', *, *, #4988, .F. ) ;
#11250 = ORIENTED_EDGE ( 'NONE', *, *, #5750, .T. ) ;
#11251 = EDGE_CURVE ( 'NONE', #3952, #10292, #2609, .T. ) ;
#11252 = LINE ( 'NONE', #9512, #7058 ) ;
#11253 = AXIS2_PLACEMENT_3D ( 'NONE', #4097, #3224, #7156 ) ;
#11254 = CARTESIAN_POINT ( 'NONE',  ( 3.309651814758565180, -5.455921364805393026, -1.000000000000000000 ) ) ;
#11255 = FACE_OUTER_BOUND ( 'NONE', #3134, .T. ) ;
#11256 = ADVANCED_FACE ( 'NONE', ( #10324 ), #9342, .F. ) ;
#11257 = ORIENTED_EDGE ( 'NONE', *, *, #10098, .F. ) ;
#11258 = DIRECTION ( 'NONE',  ( -1.000000000000000000, -0.000000000000000000, -0.000000000000000000 ) ) ;
#11259 = VECTOR ( 'NONE', #6334, 1000.000000000000000 ) ;
#11260 = DIRECTION ( 'NONE',  ( -1.000000000000000000, -0.000000000000000000, -0.000000000000000000 ) ) ;
#11261 = CARTESIAN_POINT ( 'NONE',  ( 4.999999999999999112, 6.283573709965571297, -19.24938187143289881 ) ) ;
#11262 = ORIENTED_EDGE ( 'NONE', *, *, #2698, .F. ) ;
#11263 = CARTESIAN_POINT ( 'NONE',  ( 4.999999999999999112, 0.000000000000000000, 0.000000000000000000 ) ) ;
#11264 = CYLINDRICAL_SURFACE ( 'NONE', #6243, 7.500000000000000000 ) ;
#11265 = ORIENTED_EDGE ( 'NONE', *, *, #3267, .T. ) ;
#11266 = EDGE_CURVE ( 'NONE', #7184, #8068, #5579, .T. ) ;
#11267 = CARTESIAN_POINT ( 'NONE',  ( -15.00000000000000000, 40.00000000000000711, 0.000000000000000000 ) ) ;
#11268 = DIRECTION ( 'NONE',  ( 0.000000000000000000, 0.000000000000000000, 1.000000000000000000 ) ) ;
#11269 = EDGE_LOOP ( 'NONE', ( #5907, #7622, #3824, #554 ) ) ;
#11270 = CARTESIAN_POINT ( 'NONE',  ( 4.999999999999999112, 0.000000000000000000, 14.24900000001425227 ) ) ;
#11271 = EDGE_CURVE ( 'NONE', #11670, #6322, #25, .T. ) ;
#11272 = AXIS2_PLACEMENT_3D ( 'NONE', #11496, #8456, #12246 ) ;
#11273 = VERTEX_POINT ( 'NONE', #9773 ) ;
#11274 = EDGE_CURVE ( 'NONE', #5710, #5423, #4208, .T. ) ;
#11275 = DIRECTION ( 'NONE',  ( -1.000000000000000000, -0.000000000000000000, -0.000000000000000000 ) ) ;
#11276 = FACE_OUTER_BOUND ( 'NONE', #12240, .T. ) ;
#11277 = DIRECTION ( 'NONE',  ( 1.000000000000000000, 0.000000000000000000, 0.000000000000000000 ) ) ;
#11278 = CARTESIAN_POINT ( 'NONE',  ( 4.999999999999999112, -5.622796541391657854, 13.09267581720865259 ) ) ;
#11279 = DIRECTION ( 'NONE',  ( 1.000000000000000000, 0.000000000000000000, 0.000000000000000000 ) ) ;
#11280 = EDGE_LOOP ( 'NONE', ( #5207, #11959, #8159, #10476 ) ) ;
#11281 = ORIENTED_EDGE ( 'NONE', *, *, #8827, .T. ) ;
#11282 = CARTESIAN_POINT ( 'NONE',  ( 4.999999999999999112, 13.09267581720866858, 5.622796541391611669 ) ) ;
#11283 = VERTEX_POINT ( 'NONE', #7665 ) ;
#11284 = CARTESIAN_POINT ( 'NONE',  ( 0.000000000000000000, -15.22291137398932470, 14.46592441914958904 ) ) ;
#11285 = SHAPE_DEFINITION_REPRESENTATION ( #3519, #588 ) ;
#11286 = ORIENTED_EDGE ( 'NONE', *, *, #8917, .F. ) ;
#11287 = PRODUCT_DEFINITION ( 'UNKNOWN', '', #255, #3022 ) ;
#11288 = DIRECTION ( 'NONE',  ( -0.000000000000000000, 1.000000000000000000, -0.000000000000000000 ) ) ;
#11289 = CYLINDRICAL_SURFACE ( 'NONE', #11351, 7.500000000000000000 ) ;
#11290 = ORIENTED_EDGE ( 'NONE', *, *, #10197, .T. ) ;
#11291 = LINE ( 'NONE', #9183, #206 ) ;
#11292 = SHAPE_REPRESENTATION ( 'angular contact ball bearing_68_iso_ISO 15 ABB - 1710 - 20,SI,NC,20_68', ( #6056 ), #6426 ) ;
#11293 = CARTESIAN_POINT ( 'NONE',  ( 0.02381023875259481032, 0.5999999999999999778, 2.905405940543879240 ) ) ;
#11294 = ORIENTED_EDGE ( 'NONE', *, *, #2273, .F. ) ;
#11295 = EDGE_CURVE ( 'NONE', #8402, #863, #5615, .T. ) ;
#11296 = EDGE_CURVE ( 'NONE', #170, #7890, #10997, .T. ) ;
#11297 = CARTESIAN_POINT ( 'NONE',  ( 50.00005079999999680, 4.769696007084728073, -1.500000000000000000 ) ) ;
#11298 = ORIENTED_EDGE ( 'NONE', *, *, #7829, .F. ) ;
#11299 = SURFACE_STYLE_FILL_AREA ( #12292 ) ;
#11300 = FACE_BOUND ( 'NONE', #5617, .T. ) ;
#11301 = EDGE_LOOP ( 'NONE', ( #10705, #4964, #2099, #1141 ) ) ;
#11302 = DIRECTION ( 'NONE',  ( 0.000000000000000000, -6.866613759067993855E-15, 1.000000000000000000 ) ) ;
#11303 = CARTESIAN_POINT ( 'NONE',  ( 33.00000000000000000, 0.000000000000000000, -41.99999999999999289 ) ) ;
#11304 = CARTESIAN_POINT ( 'NONE',  ( 51.00000000000000000, 3.500000000000001332, -45.49999999999998579 ) ) ;
#11305 = CARTESIAN_POINT ( 'NONE',  ( 0.000000000000000000, -11.41582255376066968, -8.527191590521194797 ) ) ;
#11306 = VERTEX_POINT ( 'NONE', #8773 ) ;
#11307 = ORIENTED_EDGE ( 'NONE', *, *, #4003, .T. ) ;
#11308 = CARTESIAN_POINT ( 'NONE',  ( 42.00000000000000000, 4.814824860968089633E-32, 0.000000000000000000 ) ) ;
#11309 = FILL_AREA_STYLE_COLOUR ( '', #631 ) ;
#11310 = CARTESIAN_POINT ( 'NONE',  ( 0.000000000000000000, 0.5192545390863916310, 0.000000000000000000 ) ) ;
#11311 = DIRECTION ( 'NONE',  ( 1.000000000000000000, 0.000000000000000000, 0.000000000000000000 ) ) ;
#11312 = ORIENTED_EDGE ( 'NONE', *, *, #6020, .T. ) ;
#11313 = CARTESIAN_POINT ( 'NONE',  ( 5.200000000000002842, 0.000000000000000000, 0.000000000000000000 ) ) ;
#11314 = SURFACE_SIDE_STYLE ('',( #1951 ) ) ;
#11315 = DIRECTION ( 'NONE',  ( 1.000000000000000000, 0.000000000000000000, 0.000000000000000000 ) ) ;
#11316 = VERTEX_POINT ( 'NONE', #3954 ) ;
#11317 = CARTESIAN_POINT ( 'NONE',  ( 4.999999999999999112, 0.000000000000000000, 0.000000000000000000 ) ) ;
#11318 = ORIENTED_EDGE ( 'NONE', *, *, #8048, .F. ) ;
#11319 = DIRECTION ( 'NONE',  ( 0.000000000000000000, 0.000000000000000000, -1.000000000000000000 ) ) ;
#11320 = DIRECTION ( 'NONE',  ( -1.000000000000000000, 0.000000000000000000, -0.000000000000000000 ) ) ;
#11321 = VERTEX_POINT ( 'NONE', #10576 ) ;
#11322 = DIRECTION ( 'NONE',  ( 1.000000000000000000, 0.000000000000000000, -0.000000000000000000 ) ) ;
#11323 = ORIENTED_EDGE ( 'NONE', *, *, #5254, .T. ) ;
#11324 = ADVANCED_FACE ( 'NONE', ( #10653 ), #2832, .F. ) ;
#11325 = FILL_AREA_STYLE_COLOUR ( '', #2575 ) ;
#11326 = LINE ( 'NONE', #3594, #2591 ) ;
#11327 = CARTESIAN_POINT ( 'NONE',  ( 26.00000000000000355, 9.184850993605147944E-16, -49.49999999999999289 ) ) ;
#11328 = ADVANCED_FACE ( 'NONE', ( #9524 ), #1085, .T. ) ;
#11329 = CARTESIAN_POINT ( 'NONE',  ( 36.00000000000000711, -3.403685371105885427, -38.61548734756097190 ) ) ;
#11330 = PLANE ( 'NONE',  #12005 ) ;
#11331 = ORIENTED_EDGE ( 'NONE', *, *, #3428, .T. ) ;
#11332 = ORIENTED_EDGE ( 'NONE', *, *, #11725, .T. ) ;
#11333 = CARTESIAN_POINT ( 'NONE',  ( 0.000000000000000000, -1.178949249685218303, -2.041999999999998039 ) ) ;
#11334 = ORIENTED_EDGE ( 'NONE', *, *, #2272, .T. ) ;
#11335 = APPLICATION_PROTOCOL_DEFINITION ( 'draft international standard', 'automotive_design', 1998, #2820 ) ;
#11336 = ORIENTED_EDGE ( 'NONE', *, *, #3644, .T. ) ;
#11337 = CARTESIAN_POINT ( 'NONE',  ( -0.1481481481481481122, -4.797713218419819903, -1.000000000000000000 ) ) ;
#11338 = DIRECTION ( 'NONE',  ( 0.000000000000000000, -0.3826834323650774028, -0.9238795325112918455 ) ) ;
#11339 = CIRCLE ( 'NONE', #2356, 9.600000000009599077 ) ;
#11340 = AXIS2_PLACEMENT_3D ( 'NONE', #10555, #9702, #6642 ) ;
#11341 = ORIENTED_EDGE ( 'NONE', *, *, #2679, .T. ) ;
#11342 = ORIENTED_EDGE ( 'NONE', *, *, #12183, .T. ) ;
#11343 = CARTESIAN_POINT ( 'NONE',  ( 0.000000000000000000, 0.000000000000000000, 0.000000000000000000 ) ) ;
#11344 = ADVANCED_FACE ( 'NONE', ( #7772 ), #2085, .F. ) ;
#11345 = ADVANCED_FACE ( 'NONE', ( #948 ), #5838, .F. ) ;
#11346 = DIRECTION ( 'NONE',  ( 0.000000000000000000, 0.000000000000000000, 1.000000000000000000 ) ) ;
#11348 = ADVANCED_FACE ( 'NONE', ( #8587 ), #5906, .T. ) ;
#11347 = FACE_OUTER_BOUND ( 'NONE', #11145, .T. ) ;
#11349 = ORIENTED_EDGE ( 'NONE', *, *, #10328, .F. ) ;
#11350 = CARTESIAN_POINT ( 'NONE',  ( 1.000000000000000000, 0.000000000000000000, 3.873645755336797780 ) ) ;
#11351 = AXIS2_PLACEMENT_3D ( 'NONE', #969, #4788, #11232 ) ;
#11352 = ORIENTED_EDGE ( 'NONE', *, *, #2670, .F. ) ;
#11353 = APPLICATION_CONTEXT ( 'automotive_design' ) ;
#11354 = AXIS2_PLACEMENT_3D ( 'NONE', #6435, #1736, #2677 ) ;
#11355 = ORIENTED_EDGE ( 'NONE', *, *, #12267, .T. ) ;
#11356 = CARTESIAN_POINT ( 'NONE',  ( 50.00005079999999680, 6.123233995736766282E-16, -5.000000000000000000 ) ) ;
#11357 = ORIENTED_EDGE ( 'NONE', *, *, #5702, .F. ) ;
#11358 = CARTESIAN_POINT ( 'NONE',  ( 4.999999999999999112, -13.17168466712939257, 15.37949036966207039 ) ) ;
#11359 = EDGE_CURVE ( 'NONE', #403, #8328, #6219, .T. ) ;
#11360 = SHAPE_REPRESENTATION ( 'spindle', ( #6056 ), #2232 ) ;
#11361 = LINE ( 'NONE', #6446, #2584 ) ;
#11362 =( GEOMETRIC_REPRESENTATION_CONTEXT ( 3 ) GLOBAL_UNCERTAINTY_ASSIGNED_CONTEXT ( ( #1920 ) ) GLOBAL_UNIT_ASSIGNED_CONTEXT ( ( #4525, #8342, #763 ) ) REPRESENTATION_CONTEXT ( 'NONE', 'WORKASPACE' ) );
#11363 = DIRECTION ( 'NONE',  ( 0.000000000000000000, 0.000000000000000000, 1.000000000000000000 ) ) ;
#11364 = CARTESIAN_POINT ( 'NONE',  ( 0.000000000000000000, 14.40062958310465469, -1.672489362011036595 ) ) ;
#11365 = ORIENTED_EDGE ( 'NONE', *, *, #1807, .T. ) ;
#11366 = ORIENTED_EDGE ( 'NONE', *, *, #8830, .T. ) ;
#11367 = CARTESIAN_POINT ( 'NONE',  ( 4.999999999999999112, 0.000000000000000000, 0.000000000000000000 ) ) ;
#11368 = SHAPE_REPRESENTATION_RELATIONSHIP ( 'NONE' , 'NONE' ,  #678, #9458 ) ;
#11369 = DIRECTION ( 'NONE',  ( 1.000000000000000000, 0.000000000000000000, 0.000000000000000000 ) ) ;
#11370 = CIRCLE ( 'NONE', #9991, 9.600000000009600853 ) ;
#11371 = CARTESIAN_POINT ( 'NONE',  ( 4.999999999999999112, 14.40062958310465469, -8.872489362018239234 ) ) ;
#11372 = ORIENTED_EDGE ( 'NONE', *, *, #4957, .T. ) ;
#11373 = LINE ( 'NONE', #9463, #2993 ) ;
#11374 = AXIS2_PLACEMENT_3D ( 'NONE', #835, #11458, #2906 ) ;
#11375 = EDGE_CURVE ( 'NONE', #11209, #1819, #2417, .T. ) ;
#11376 = MECHANICAL_DESIGN_GEOMETRIC_PRESENTATION_REPRESENTATION (  '', ( #7408 ), #9007 ) ;
#11377 = FILL_AREA_STYLE_COLOUR ( '', #7614 ) ;
#11378 = DIRECTION ( 'NONE',  ( 0.000000000000000000, 0.000000000000000000, -1.000000000000000000 ) ) ;
#11379 = CIRCLE ( 'NONE', #10788, 7.200000000007201528 ) ;
#11380 = AXIS2_PLACEMENT_3D ( 'NONE', #7561, #6506, #10248 ) ;
#11381 = CARTESIAN_POINT ( 'NONE',  ( 0.000000000000000000, 0.000000000000000000, 0.000000000000000000 ) ) ;
#11382 = FACE_OUTER_BOUND ( 'NONE', #4791, .T. ) ;
#11383 = ORIENTED_EDGE ( 'NONE', *, *, #10953, .F. ) ;
#11384 = CARTESIAN_POINT ( 'NONE',  ( 46.00000000000000000, 5.000000000000004441, -41.99999999999998579 ) ) ;
#11385 = CARTESIAN_POINT ( 'NONE',  ( 3.309651814758564736, -5.455921364805393026, 0.000000000000000000 ) ) ;
#11386 = ORIENTED_EDGE ( 'NONE', *, *, #10217, .F. ) ;
#11387 = DIRECTION ( 'NONE',  ( -1.000000000000000000, 0.000000000000000000, 0.000000000000000000 ) ) ;
#11388 = UNCERTAINTY_MEASURE_WITH_UNIT (LENGTH_MEASURE( 1.000000000000000082E-05 ), #12161, 'distance_accuracy_value', 'NONE');
#11389 = ORIENTED_EDGE ( 'NONE', *, *, #804, .T. ) ;
#11390 = AXIS2_PLACEMENT_3D ( 'NONE', #9924, #1480, #2341 ) ;
#11391 = VECTOR ( 'NONE', #4046, 1000.000000000000000 ) ;
#11392 = DIRECTION ( 'NONE',  ( 1.000000000000000000, 0.000000000000000000, 0.000000000000000000 ) ) ;
#11393 = DIRECTION ( 'NONE',  ( 0.000000000000000000, 0.000000000000000000, 1.000000000000000000 ) ) ;
#11394 = LINE ( 'NONE', #9410, #361 ) ;
#11395 = CIRCLE ( 'NONE', #3651, 14.24900000001425049 ) ;
#11396 = CARTESIAN_POINT ( 'NONE',  ( 51.00000000000000000, -3.499999999999998668, -45.49999999999998579 ) ) ;
#11397 = CARTESIAN_POINT ( 'NONE',  ( 0.000000000000000000, 0.000000000000000000, 14.24900000001425227 ) ) ;
#11398 = CIRCLE ( 'NONE', #1222, 5.000000000000000000 ) ;
#11399 = AXIS2_PLACEMENT_3D ( 'NONE', #2518, #1525, #11889 ) ;
#11400 = ORIENTED_EDGE ( 'NONE', *, *, #9544, .T. ) ;
#11401 = ORIENTED_EDGE ( 'NONE', *, *, #8398, .F. ) ;
#11402 = DIRECTION ( 'NONE',  ( 1.000000000000000000, -0.000000000000000000, -0.000000000000000000 ) ) ;
#11403 = CIRCLE ( 'NONE', #4024, 27.00000000002699707 ) ;
#11404 = ORIENTED_EDGE ( 'NONE', *, *, #8242, .T. ) ;
#11405 = CARTESIAN_POINT ( 'NONE',  ( -36.00000000000000000, 30.00000000000000711, -19.99999999999998934 ) ) ;
#11406 = EDGE_CURVE ( 'NONE', #8093, #11316, #9235, .T. ) ;
#11407 = PRODUCT_CONTEXT ( 'NONE', #5206, 'mechanical' ) ;
#11408 = VERTEX_POINT ( 'NONE', #84 ) ;
#11409 = FACE_OUTER_BOUND ( 'NONE', #1124, .T. ) ;
#11410 = ADVANCED_FACE ( 'NONE', ( #7845 ), #11641, .F. ) ;
#11411 = CARTESIAN_POINT ( 'NONE',  ( 0.000000000000000000, 20.41639017900859443, -4.916402349214656020 ) ) ;
#11412 = CIRCLE ( 'NONE', #1837, 9.600000000009602630 ) ;
#11413 = CIRCLE ( 'NONE', #634, 9.600000000009599077 ) ;
#11414 = ORIENTED_EDGE ( 'NONE', *, *, #8929, .F. ) ;
#11415 = VECTOR ( 'NONE', #2694, 1000.000000000000000 ) ;
#11416 = EDGE_LOOP ( 'NONE', ( #2882, #1865 ) ) ;
#11417 = CARTESIAN_POINT ( 'NONE',  ( 0.000000000000000000, 0.000000000000000000, 0.000000000000000000 ) ) ;
#11418 = PLANE ( 'NONE',  #5419 ) ;
#11419 = CARTESIAN_POINT ( 'NONE',  ( -1.067261513540418427E-16, 0.5999999999999998668, 2.765611175118570575 ) ) ;
#11420 = CARTESIAN_POINT ( 'NONE',  ( 17.00000000000000000, 0.000000000000000000, 2.055000000000000160 ) ) ;
#11421 = EDGE_LOOP ( 'NONE', ( #9141, #347, #1086, #6555 ) ) ;
#11422 = CARTESIAN_POINT ( 'NONE',  ( -20.63749999999999929, 0.000000000000000000, 0.000000000000000000 ) ) ;
#11423 = AXIS2_PLACEMENT_3D ( 'NONE', #11263, #9284, #2700 ) ;
#11424 = ORIENTED_EDGE ( 'NONE', *, *, #3444, .T. ) ;
#11425 = AXIS2_PLACEMENT_3D ( 'NONE', #8703, #3942, #7758 ) ;
#11426 = EDGE_CURVE ( 'NONE', #4747, #8068, #268, .T. ) ;
#11427 = CIRCLE ( 'NONE', #3247, 9.600000000009600853 ) ;
#11428 = ORIENTED_EDGE ( 'NONE', *, *, #9679, .T. ) ;
#11429 = CARTESIAN_POINT ( 'NONE',  ( 4.999999999999999112, 20.18872947935930995, 1.561154383803294410 ) ) ;
#11430 = EDGE_CURVE ( 'NONE', #11755, #114, #10817, .T. ) ;
#11431 = ORIENTED_EDGE ( 'NONE', *, *, #7171, .F. ) ;
#11432 = DIRECTION ( 'NONE',  ( 1.000000000000000000, 0.000000000000000000, 0.000000000000000000 ) ) ;
#11433 = ADVANCED_FACE ( 'NONE', ( #6662 ), #10461, .T. ) ;
#11434 = AXIS2_PLACEMENT_3D ( 'NONE', #7358, #9175, #4479 ) ;
#11435 = DIRECTION ( 'NONE',  ( -1.000000000000000000, 0.000000000000000000, 0.000000000000000000 ) ) ;
#11436 = CARTESIAN_POINT ( 'NONE',  ( 0.000000000000000000, 26.33508479058329499, -5.955107813822217544 ) ) ;
#11437 = CARTESIAN_POINT ( 'NONE',  ( -20.63749999999999574, 0.000000000000000000, 0.000000000000000000 ) ) ;
#11438 = ORIENTED_EDGE ( 'NONE', *, *, #5422, .F. ) ;
#11439 = DIRECTION ( 'NONE',  ( -1.000000000000000000, -0.000000000000000000, -0.000000000000000000 ) ) ;
#11440 = DIRECTION ( 'NONE',  ( 0.000000000000000000, 0.000000000000000000, -1.000000000000000000 ) ) ;
#11441 = DIRECTION ( 'NONE',  ( 0.000000000000000000, 0.000000000000000000, -1.000000000000000000 ) ) ;
#11442 = AXIS2_PLACEMENT_3D ( 'NONE', #12176, #1886, #935 ) ;
#11443 = ORIENTED_EDGE ( 'NONE', *, *, #9401, .T. ) ;
#11444 = FACE_OUTER_BOUND ( 'NONE', #6179, .T. ) ;
#11445 = DIRECTION ( 'NONE',  ( 0.000000000000000000, 0.000000000000000000, -1.000000000000000000 ) ) ;
#11446 = CARTESIAN_POINT ( 'NONE',  ( 37.00000000000000711, 3.277848209564066639, -38.49347592122088457 ) ) ;
#11447 = DIRECTION ( 'NONE',  ( 0.000000000000000000, 1.000000000000000000, 3.491481338843133750E-15 ) ) ;
#11448 = DIRECTION ( 'NONE',  ( 0.000000000000000000, 0.000000000000000000, -1.000000000000000000 ) ) ;
#11449 = VERTEX_POINT ( 'NONE', #11818 ) ;
#11450 = LINE ( 'NONE', #7957, #11553 ) ;
#11451 = EDGE_CURVE ( 'NONE', #1747, #8607, #4032, .T. ) ;
#11452 = DIRECTION ( 'NONE',  ( 0.000000000000000000, 0.000000000000000000, 1.000000000000000000 ) ) ;
#11453 = ADVANCED_FACE ( 'NONE', ( #8028 ), #1375, .F. ) ;
#11454 = ORIENTED_EDGE ( 'NONE', *, *, #2944, .T. ) ;
#11455 = CARTESIAN_POINT ( 'NONE',  ( 4.999999999999999112, 0.000000000000000000, 0.000000000000000000 ) ) ;
#11456 = VERTEX_POINT ( 'NONE', #9899 ) ;
#11457 = VECTOR ( 'NONE', #8051, 1000.000000000000000 ) ;
#11458 = DIRECTION ( 'NONE',  ( -1.000000000000000000, -3.903127820947815962E-18, 0.000000000000000000 ) ) ;
#11459 = DIRECTION ( 'NONE',  ( -1.000000000000000000, 0.000000000000000000, 0.000000000000000000 ) ) ;
#11460 = LINE ( 'NONE', #3032, #7963 ) ;
#11461 = CARTESIAN_POINT ( 'NONE',  ( 2.399999999999999467, 0.000000000000000000, 2.000000000000000000 ) ) ;
#11462 = CARTESIAN_POINT ( 'NONE',  ( 4.999999999999999112, 0.000000000000000000, 0.000000000000000000 ) ) ;
#11463 = ORIENTED_EDGE ( 'NONE', *, *, #1205, .T. ) ;
#11464 = ORIENTED_EDGE ( 'NONE', *, *, #11174, .F. ) ;
#11465 = CIRCLE ( 'NONE', #5892, 9.600000000009600853 ) ;
#11466 = EDGE_LOOP ( 'NONE', ( #1959, #3312, #9851, #9328 ) ) ;
#11467 = DIRECTION ( 'NONE',  ( 0.000000000000000000, 0.000000000000000000, 1.000000000000000000 ) ) ;
#11468 = CONTEXT_DEPENDENT_SHAPE_REPRESENTATION ( #5864, #10916 ) ;
#11469 = ORIENTED_EDGE ( 'NONE', *, *, #108, .T. ) ;
#11470 = VECTOR ( 'NONE', #938, 1000.000000000000000 ) ;
#11471 = EDGE_LOOP ( 'NONE', ( #5986, #10282, #7588, #1372 ) ) ;
#11472 = ORIENTED_EDGE ( 'NONE', *, *, #4457, .F. ) ;
#11473 = DIRECTION ( 'NONE',  ( -1.000000000000000000, 0.000000000000000000, 0.000000000000000000 ) ) ;
#11474 = DIRECTION ( 'NONE',  ( -1.000000000000000000, 0.000000000000000000, -0.000000000000000000 ) ) ;
#11475 = LINE ( 'NONE', #9618, #7429 ) ;
#11476 = CARTESIAN_POINT ( 'NONE',  ( -26.00000000000000355, 0.000000000000000000, 0.000000000000000000 ) ) ;
#11477 = EDGE_CURVE ( 'NONE', #6450, #3193, #448, .T. ) ;
#11478 = VERTEX_POINT ( 'NONE', #3279 ) ;
#11479 = CARTESIAN_POINT ( 'NONE',  ( 1.600000000000000089, 0.000000000000000000, 0.000000000000000000 ) ) ;
#11480 = VERTEX_POINT ( 'NONE', #11695 ) ;
#11481 = CIRCLE ( 'NONE', #2695, 2.149999999999999023 ) ;
#11482 = SHAPE_REPRESENTATION_RELATIONSHIP ( 'NONE' , 'NONE' ,  #10563, #8868 ) ;
#11483 = ORIENTED_EDGE ( 'NONE', *, *, #4109, .F. ) ;
#11484 = FACE_OUTER_BOUND ( 'NONE', #7694, .T. ) ;
#11485 = VERTEX_POINT ( 'NONE', #2197 ) ;
#11486 = CARTESIAN_POINT ( 'NONE',  ( 4.999999999999999112, 8.035066368449204077, 14.88411597386731877 ) ) ;
#11487 = DIRECTION ( 'NONE',  ( -1.000000000000000000, -0.000000000000000000, -0.000000000000000000 ) ) ;
#11488 = EDGE_CURVE ( 'NONE', #8676, #12066, #5028, .T. ) ;
#11489 = EDGE_CURVE ( 'NONE', #10639, #3355, #8097, .T. ) ;
#11490 = DIRECTION ( 'NONE',  ( 0.000000000000000000, 0.000000000000000000, -1.000000000000000000 ) ) ;
#11491 = CARTESIAN_POINT ( 'NONE',  ( 37.00000000000000711, -3.606021680338235225, -38.83193945118931367 ) ) ;
#11492 = EDGE_CURVE ( 'NONE', #7335, #7692, #831, .T. ) ;
#11493 = VERTEX_POINT ( 'NONE', #5133 ) ;
#11494 = DIRECTION ( 'NONE',  ( 0.000000000000000000, 0.000000000000000000, -1.000000000000000000 ) ) ;
#11495 = FACE_OUTER_BOUND ( 'NONE', #5289, .T. ) ;
#11496 = CARTESIAN_POINT ( 'NONE',  ( -20.63749999999999929, 0.000000000000000000, 0.000000000000000000 ) ) ;
#11497 = VERTEX_POINT ( 'NONE', #6085 ) ;
#11498 = DIRECTION ( 'NONE',  ( 0.000000000000000000, 0.000000000000000000, -1.000000000000000000 ) ) ;
#11499 = LINE ( 'NONE', #6655, #8208 ) ;
#11500 = DIRECTION ( 'NONE',  ( 0.000000000000000000, 0.000000000000000000, 1.000000000000000000 ) ) ;
#11501 = ADVANCED_FACE ( 'NONE', ( #9144 ), #1319, .T. ) ;
#11502 = ADVANCED_FACE ( 'NONE', ( #5080 ), #507, .T. ) ;
#11503 = CARTESIAN_POINT ( 'NONE',  ( 2.499999999999998668, -15.22291137398932470, 14.46592441914958904 ) ) ;
#11504 = CARTESIAN_POINT ( 'NONE',  ( 0.000000000000000000, -14.88411597386734897, 8.035066368449154339 ) ) ;
#11505 = EDGE_CURVE ( 'NONE', #2177, #9383, #1453, .T. ) ;
#11506 = VERTEX_POINT ( 'NONE', #1266 ) ;
#11507 = CARTESIAN_POINT ( 'NONE',  ( 0.000000000000000000, 0.000000000000000000, 0.000000000000000000 ) ) ;
#11508 = CARTESIAN_POINT ( 'NONE',  ( 0.000000000000000000, 0.000000000000000000, 0.000000000000000000 ) ) ;
#11509 = EDGE_LOOP ( 'NONE', ( #11977, #6484, #3096, #10984 ) ) ;
#11510 = LINE ( 'NONE', #4836, #96 ) ;
#11511 = UNCERTAINTY_MEASURE_WITH_UNIT (LENGTH_MEASURE( 1.000000000000000082E-05 ), #2556, 'distance_accuracy_value', 'NONE');
#11512 = ORIENTED_EDGE ( 'NONE', *, *, #4661, .T. ) ;
#11513 = EDGE_CURVE ( 'NONE', #7220, #11850, #4837, .T. ) ;
#11514 = EDGE_CURVE ( 'NONE', #922, #1183, #9951, .T. ) ;
#11515 = CARTESIAN_POINT ( 'NONE',  ( 0.000000000000000000, 8.572527594031473190E-16, -7.000000000000000000 ) ) ;
#11516 = CARTESIAN_POINT ( 'NONE',  ( -36.00000000000000000, 0.000000000000000000, 0.000000000000000000 ) ) ;
#11517 = LINE ( 'NONE', #8861, #5235 ) ;
#11518 = DIRECTION ( 'NONE',  ( 0.000000000000000000, 0.000000000000000000, 1.000000000000000000 ) ) ;
#11519 = ORIENTED_EDGE ( 'NONE', *, *, #3413, .F. ) ;
#11520 = ORIENTED_EDGE ( 'NONE', *, *, #4781, .T. ) ;
#11521 = CARTESIAN_POINT ( 'NONE',  ( 4.999999999999999112, -16.90755573046745752, -0.4834863907627537372 ) ) ;
#11522 = VERTEX_POINT ( 'NONE', #5194 ) ;
#11523 = FACE_OUTER_BOUND ( 'NONE', #7880, .T. ) ;
#11524 = ORIENTED_EDGE ( 'NONE', *, *, #6811, .F. ) ;
#11525 = EDGE_CURVE ( 'NONE', #10109, #3666, #2266, .T. ) ;
#11526 = ORIENTED_EDGE ( 'NONE', *, *, #430, .F. ) ;
#11527 = VERTEX_POINT ( 'NONE', #9026 ) ;
#11528 = DIRECTION ( 'NONE',  ( -1.000000000000000000, -0.000000000000000000, -0.000000000000000000 ) ) ;
#11529 = DIRECTION ( 'NONE',  ( 0.000000000000000000, 0.5000000000000008882, -0.8660254037844381525 ) ) ;
#11530 = CARTESIAN_POINT ( 'NONE',  ( 2.500000000000000000, 1.768423874527824902, 1.020999999999999019 ) ) ;
#11531 = DIRECTION ( 'NONE',  ( -1.000000000000000000, 0.000000000000000000, 0.000000000000000000 ) ) ;
#11532 = ORIENTED_EDGE ( 'NONE', *, *, #4396, .T. ) ;
#11533 = DIRECTION ( 'NONE',  ( -1.000000000000000000, 0.000000000000000000, -0.000000000000000000 ) ) ;
#11534 = VERTEX_POINT ( 'NONE', #8958 ) ;
#11535 =( NAMED_UNIT ( * ) SI_UNIT ( $, .STERADIAN. ) SOLID_ANGLE_UNIT ( ) );
#11536 = EDGE_LOOP ( 'NONE', ( #5627, #10289 ) ) ;
#11538 = DIRECTION ( 'NONE',  ( 0.000000000000000000, 0.7900737791495477946, 0.6130117645692876316 ) ) ;
#11537 = CIRCLE ( 'NONE', #12338, 20.24900000002024569 ) ;
#11539 = ORIENTED_EDGE ( 'NONE', *, *, #2489, .F. ) ;
#11540 = PLANE ( 'NONE',  #3764 ) ;
#11541 = AXIS2_PLACEMENT_3D ( 'NONE', #4716, #5775, #9534 ) ;
#11542 = CARTESIAN_POINT ( 'NONE',  ( 0.000000000000000000, 0.000000000000000000, 0.000000000000000000 ) ) ;
#11543 = CIRCLE ( 'NONE', #10951, 4.000000000000003553 ) ;
#11544 = ORIENTED_EDGE ( 'NONE', *, *, #1051, .T. ) ;
#11545 = CARTESIAN_POINT ( 'NONE',  ( -10.00000000000000000, 0.000000000000000000, 0.000000000000000000 ) ) ;
#11546 = CARTESIAN_POINT ( 'NONE',  ( 26.00000000000000355, 1.456773409934505593E-31, -36.99999999999998579 ) ) ;
#11547 = EDGE_LOOP ( 'NONE', ( #6275, #204, #7809, #907 ) ) ;
#11548 = LINE ( 'NONE', #4816, #9650 ) ;
#11549 = DIRECTION ( 'NONE',  ( -0.000000000000000000, 1.000000000000000000, -0.000000000000000000 ) ) ;
#11550 = EDGE_CURVE ( 'NONE', #5230, #3761, #4191, .T. ) ;
#11551 = ORIENTED_EDGE ( 'NONE', *, *, #6261, .F. ) ;
#11552 = FACE_OUTER_BOUND ( 'NONE', #4730, .T. ) ;
#11553 = VECTOR ( 'NONE', #5132, 1000.000000000000000 ) ;
#11554 = CIRCLE ( 'NONE', #7976, 40.00000000000000711 ) ;
#11555 = EDGE_CURVE ( 'NONE', #1347, #3862, #5623, .T. ) ;
#11556 = VECTOR ( 'NONE', #10218, 1000.000000000000000 ) ;
#11557 = DIRECTION ( 'NONE',  ( -1.000000000000000000, 0.000000000000000000, 0.000000000000000000 ) ) ;
#11558 = DIRECTION ( 'NONE',  ( 0.000000000000000000, 0.000000000000000000, -1.000000000000000000 ) ) ;
#11559 = FACE_OUTER_BOUND ( 'NONE', #10830, .T. ) ;
#11560 = AXIS2_PLACEMENT_3D ( 'NONE', #4280, #3232, #6292 ) ;
#11561 = AXIS2_PLACEMENT_3D ( 'NONE', #5180, #10814, #9012 ) ;
#11562 = ORIENTED_EDGE ( 'NONE', *, *, #4166, .F. ) ;
#11563 = CYLINDRICAL_SURFACE ( 'NONE', #2983, 7.200000000007202416 ) ;
#11564 = CARTESIAN_POINT ( 'NONE',  ( -15.00000000000000000, 44.00000000000001421, 0.000000000000000000 ) ) ;
#11565 = VECTOR ( 'NONE', #4587, 1000.000000000000000 ) ;
#11566 = EDGE_LOOP ( 'NONE', ( #6006, #8467, #10340, #6761, #3755, #202, #2095, #4171, #7108, #4597, #10245, #2086, #3863, #5164, #6494, #3289, #7737, #10863, #10719, #7745, #5794, #4894, #10080, #2876, #952, #5836, #928, #5730, #4413, #1584, #10629, #11693, #11519, #6799, #2916, #141, #3150, #2509, #12152, #10377, #8112, #9129, #2817, #109, #10441, #5355, #4666, #7129, #9499, #821, #2195, #7487, #4921 ) ) ;
#11567 = DIRECTION ( 'NONE',  ( 0.000000000000000000, 0.000000000000000000, 1.000000000000000000 ) ) ;
#11568 = EDGE_CURVE ( 'NONE', #3494, #1873, #6200, .T. ) ;
#11569 = EDGE_LOOP ( 'NONE', ( #6598, #12033, #3262, #6284 ) ) ;
#11570 = ADVANCED_FACE ( 'NONE', ( #3697 ), #9274, .T. ) ;
#11571 = ADVANCED_FACE ( 'NONE', ( #3512 ), #11184, .T. ) ;
#11572 = ADVANCED_FACE ( 'NONE', ( #12245 ), #10373, .T. ) ;
#11573 = VECTOR ( 'NONE', #4382, 1000.000000000000000 ) ;
#11574 = VECTOR ( 'NONE', #10920, 1000.000000000000000 ) ;
#11575 = FACE_OUTER_BOUND ( 'NONE', #12112, .T. ) ;
#11576 = DIRECTION ( 'NONE',  ( -1.000000000000000000, 0.000000000000000000, -0.000000000000000000 ) ) ;
#11577 = DIRECTION ( 'NONE',  ( 0.000000000000000000, 0.000000000000000000, -1.000000000000000000 ) ) ;
#11578 = DIRECTION ( 'NONE',  ( -0.000000000000000000, 0.000000000000000000, 1.000000000000000000 ) ) ;
#11579 = ORIENTED_EDGE ( 'NONE', *, *, #12100, .F. ) ;
#11580 = DIRECTION ( 'NONE',  ( -1.000000000000000000, -0.000000000000000000, -0.000000000000000000 ) ) ;
#11581 = ORIENTED_EDGE ( 'NONE', *, *, #1493, .T. ) ;
#11582 = PRESENTATION_STYLE_ASSIGNMENT (( #154 ) ) ;
#11583 = CONTEXT_DEPENDENT_SHAPE_REPRESENTATION ( #1143, #7835 ) ;
#11584 = EDGE_CURVE ( 'NONE', #6497, #5098, #11208, .T. ) ;
#11585 = AXIS2_PLACEMENT_3D ( 'NONE', #261, #6901, #8765 ) ;
#11586 = VERTEX_POINT ( 'NONE', #1816 ) ;
#11587 = AXIS2_PLACEMENT_3D ( 'NONE', #11343, #2864, #4793 ) ;
#11588 = APPLICATION_CONTEXT ( 'automotive_design' ) ;
#11589 = VERTEX_POINT ( 'NONE', #6455 ) ;
#11590 = PRESENTATION_LAYER_ASSIGNMENT (  '', '', ( #6011 ) ) ;
#11591 = ORIENTED_EDGE ( 'NONE', *, *, #3642, .T. ) ;
#11592 = VECTOR ( 'NONE', #6401, 1000.000000000000000 ) ;
#11593 = DIRECTION ( 'NONE',  ( 1.000000000000000000, 0.000000000000000000, 0.000000000000000000 ) ) ;
#11594 = DIRECTION ( 'NONE',  ( -1.000000000000000000, 0.000000000000000000, -0.000000000000000000 ) ) ;
#11595 = AXIS2_PLACEMENT_3D ( 'NONE', #9978, #9059, #294 ) ;
#11596 = AXIS2_PLACEMENT_3D ( 'NONE', #11093, #5347, #8344 ) ;
#11597 = AXIS2_PLACEMENT_3D ( 'NONE', #1297, #5111, #2113 ) ;
#11598 = DIRECTION ( 'NONE',  ( -1.000000000000000000, -0.000000000000000000, -0.000000000000000000 ) ) ;
#11599 = CARTESIAN_POINT ( 'NONE',  ( 2.000000000000000000, -6.429618962271402616, -1.000000000000000000 ) ) ;
#11600 = ORIENTED_EDGE ( 'NONE', *, *, #3973, .F. ) ;
#11601 = DIRECTION ( 'NONE',  ( 0.000000000000000000, 0.000000000000000000, -1.000000000000000000 ) ) ;
#11602 = EDGE_LOOP ( 'NONE', ( #10527, #3352, #6310, #1542 ) ) ;
#11603 = EDGE_CURVE ( 'NONE', #8263, #9876, #9035, .T. ) ;
#11605 = EDGE_CURVE ( 'NONE', #7419, #6113, #8431, .T. ) ;
#11604 = VERTEX_POINT ( 'NONE', #10312 ) ;
#11606 = AXIS2_PLACEMENT_3D ( 'NONE', #10105, #1532, #7240 ) ;
#11607 = PLANE ( 'NONE',  #3622 ) ;
#11608 = AXIS2_PLACEMENT_3D ( 'NONE', #2506, #6327, #9205 ) ;
#11609 = PRODUCT_DEFINITION_SHAPE ( 'NONE', 'NONE',  #9994 ) ;
#11610 = AXIS2_PLACEMENT_3D ( 'NONE', #11462, #8790, #2912 ) ;
#11611 = ORIENTED_EDGE ( 'NONE', *, *, #1171, .F. ) ;
#11612 = DIRECTION ( 'NONE',  ( 0.000000000000000000, 0.8660254037844380415, -0.5000000000000012212 ) ) ;
#11613 = AXIS2_PLACEMENT_3D ( 'NONE', #12119, #1636, #4567 ) ;
#11614 = DIRECTION ( 'NONE',  ( -1.000000000000000000, -0.000000000000000000, -0.000000000000000000 ) ) ;
#11615 = PRESENTATION_LAYER_ASSIGNMENT (  '', '', ( #7846 ) ) ;
#11616 = CIRCLE ( 'NONE', #5433, 8.099999999999999645 ) ;
#11617 = AXIS2_PLACEMENT_3D ( 'NONE', #10860, #6112, #9173 ) ;
#11618 = ORIENTED_EDGE ( 'NONE', *, *, #127, .F. ) ;
#11619 = AXIS2_PLACEMENT_3D ( 'NONE', #9218, #5335, #4575 ) ;
#11620 = DIRECTION ( 'NONE',  ( -1.000000000000000000, -0.000000000000000000, -0.000000000000000000 ) ) ;
#11621 = FACE_OUTER_BOUND ( 'NONE', #3975, .T. ) ;
#11622 = ORIENTED_EDGE ( 'NONE', *, *, #5468, .F. ) ;
#11623 = CARTESIAN_POINT ( 'NONE',  ( 1.500000000000001332, 0.000000000000000000, 0.000000000000000000 ) ) ;
#11624 = FILL_AREA_STYLE_COLOUR ( '', #9830 ) ;
#11625 = CARTESIAN_POINT ( 'NONE',  ( 4.999999999999999112, 0.000000000000000000, 0.000000000000000000 ) ) ;
#11626 = DIRECTION ( 'NONE',  ( 0.000000000000000000, 0.000000000000000000, 1.000000000000000000 ) ) ;
#11627 = VERTEX_POINT ( 'NONE', #8454 ) ;
#11628 = CARTESIAN_POINT ( 'NONE',  ( 4.999999999999999112, 0.000000000000000000, 0.000000000000000000 ) ) ;
#11629 = AXIS2_PLACEMENT_3D ( 'NONE', #5299, #9121, #849 ) ;
#11630 = CIRCLE ( 'NONE', #4237, 27.00000000002699707 ) ;
#11631 = CIRCLE ( 'NONE', #8257, 7.399999999999999467 ) ;
#11632 = CIRCLE ( 'NONE', #7858, 2.149999999999999023 ) ;
#11633 = CARTESIAN_POINT ( 'NONE',  ( 0.000000000000000000, 2.791921004064247480, 22.37914155802286942 ) ) ;
#11634 = DIRECTION ( 'NONE',  ( -0.000000000000000000, 0.000000000000000000, 1.000000000000000000 ) ) ;
#11635 = FACE_OUTER_BOUND ( 'NONE', #6526, .T. ) ;
#11636 = DIRECTION ( 'NONE',  ( 0.000000000000000000, 0.000000000000000000, 1.000000000000000000 ) ) ;
#11637 = ORIENTED_EDGE ( 'NONE', *, *, #7878, .T. ) ;
#11638 = EDGE_CURVE ( 'NONE', #4328, #7808, #9387, .T. ) ;
#11639 = PLANE ( 'NONE',  #4786 ) ;
#11640 = AXIS2_PLACEMENT_3D ( 'NONE', #11123, #10082, #6199 ) ;
#11641 = CYLINDRICAL_SURFACE ( 'NONE', #3840, 2.000000000000000000 ) ;
#11642 = EDGE_LOOP ( 'NONE', ( #10430, #576, #9271, #518 ) ) ;
#11643 = DIRECTION ( 'NONE',  ( 1.000000000000000000, 0.000000000000000000, 0.000000000000000000 ) ) ;
#11644 = PRODUCT_DEFINITION_CONTEXT ( 'detailed design', #8815, 'design' ) ;
#11645 = ORIENTED_EDGE ( 'NONE', *, *, #6224, .F. ) ;
#11646 = CARTESIAN_POINT ( 'NONE',  ( 45.00000000000001421, 4.770489558936308102E-18, -41.99999999999998579 ) ) ;
#11647 = CIRCLE ( 'NONE', #274, 6.000000000000005329 ) ;
#11648 = DIRECTION ( 'NONE',  ( -1.000000000000000000, 0.000000000000000000, 0.000000000000000000 ) ) ;
#11649 = CARTESIAN_POINT ( 'NONE',  ( 36.00000000000000000, 3.061616997868383141E-16, -39.49999999999999289 ) ) ;
#11650 = EDGE_CURVE ( 'NONE', #9343, #7721, #744, .T. ) ;
#11651 = CARTESIAN_POINT ( 'NONE',  ( 36.00000000000000711, -3.756272583685665190, -38.69993692832219523 ) ) ;
#11652 = PLANE ( 'NONE',  #10820 ) ;
#11653 = EDGE_LOOP ( 'NONE', ( #8339, #11114, #9257, #11707, #10225, #6307, #5597, #7738, #5895, #5173, #1095, #1973, #10870, #12130, #4410, #12316 ) ) ;
#11654 = EDGE_CURVE ( 'NONE', #12228, #11003, #3245, .T. ) ;
#11655 = EDGE_CURVE ( 'NONE', #777, #4273, #11073, .T. ) ;
#11656 = ORIENTED_EDGE ( 'NONE', *, *, #8255, .T. ) ;
#11657 = CARTESIAN_POINT ( 'NONE',  ( 51.00000000000000711, 50.00000000000000711, -46.00000000000000000 ) ) ;
#11658 = CIRCLE ( 'NONE', #6688, 9.600000000009604406 ) ;
#11659 = ORIENTED_EDGE ( 'NONE', *, *, #4021, .T. ) ;
#11660 = DIRECTION ( 'NONE',  ( -1.000000000000000000, 0.000000000000000000, 0.000000000000000000 ) ) ;
#11661 = VERTEX_POINT ( 'NONE', #1695 ) ;
#11662 = FACE_BOUND ( 'NONE', #4300, .T. ) ;
#11663 = CARTESIAN_POINT ( 'NONE',  ( -3.206358518536427241E-14, 0.5999999999999998668, -2.905281953981669218 ) ) ;
#11664 = CIRCLE ( 'NONE', #3299, 0.2500000000000002220 ) ;
#11665 = DIRECTION ( 'NONE',  ( 0.000000000000000000, 0.000000000000000000, 1.000000000000000000 ) ) ;
#11666 = CARTESIAN_POINT ( 'NONE',  ( 0.000000000000000000, 46.00000000000001421, -37.99999999999999289 ) ) ;
#11667 = ORIENTED_EDGE ( 'NONE', *, *, #6519, .F. ) ;
#11668 = PRODUCT_DEFINITION ( 'UNKNOWN', '', #11819, #8032 ) ;
#11669 = ORIENTED_EDGE ( 'NONE', *, *, #9151, .T. ) ;
#11670 = VERTEX_POINT ( 'NONE', #12178 ) ;
#11671 = FACE_OUTER_BOUND ( 'NONE', #6378, .T. ) ;
#11672 = CIRCLE ( 'NONE', #7701, 2.041999999999999815 ) ;
#11673 = ORIENTED_EDGE ( 'NONE', *, *, #11555, .T. ) ;
#11674 = CARTESIAN_POINT ( 'NONE',  ( -3.309651814758565180, -5.455921364805393026, -1.000000000000000000 ) ) ;
#11675 = ADVANCED_BREP_SHAPE_REPRESENTATION ( '', ( #8751, #6056 ), #12194 ) ;
#11676 = CARTESIAN_POINT ( 'NONE',  ( 46.00000000000000000, 3.183245106666227286, -38.14423151746819229 ) ) ;
#11677 = EDGE_CURVE ( 'NONE', #6198, #6377, #2557, .T. ) ;
#11678 = EDGE_CURVE ( 'NONE', #394, #10459, #4447, .T. ) ;
#11679 = VERTEX_POINT ( 'NONE', #4637 ) ;
#11680 = AXIS2_PLACEMENT_3D ( 'NONE', #490, #3555, #1498 ) ;
#11681 = CYLINDRICAL_SURFACE ( 'NONE', #3178, 27.00000000002699707 ) ;
#11682 = DIRECTION ( 'NONE',  ( -1.000000000000000000, 0.000000000000000000, 0.000000000000000000 ) ) ;
#11683 = ORIENTED_EDGE ( 'NONE', *, *, #7763, .F. ) ;
#11684 = FILL_AREA_STYLE_COLOUR ( '', #1677 ) ;
#11685 = DIRECTION ( 'NONE',  ( 4.000869187770762975E-18, 0.8386705679454229401, 0.5446390350150287496 ) ) ;
#11686 = CARTESIAN_POINT ( 'NONE',  ( 0.1920286436967153787, 0.000000000000000000, 5.525000000000000355 ) ) ;
#11687 = ORIENTED_EDGE ( 'NONE', *, *, #979, .T. ) ;
#11688 = CARTESIAN_POINT ( 'NONE',  ( 1.000000000000000000, 0.000000000000000000, 0.000000000000000000 ) ) ;
#11689 = DIRECTION ( 'NONE',  ( 0.000000000000000000, 0.9238795325112850731, 0.3826834323650938896 ) ) ;
#11690 = DIRECTION ( 'NONE',  ( -1.000000000000000000, 0.000000000000000000, 0.000000000000000000 ) ) ;
#11691 = CARTESIAN_POINT ( 'NONE',  ( 4.999999999999999112, -5.622796541391657854, 13.09267581720865259 ) ) ;
#11692 = DIRECTION ( 'NONE',  ( 0.000000000000000000, -1.000000000000000000, -1.047444401652940007E-14 ) ) ;
#11693 = ORIENTED_EDGE ( 'NONE', *, *, #725, .F. ) ;
#11694 = CARTESIAN_POINT ( 'NONE',  ( 4.999999999999999112, 15.37949036966211835, 13.17168466712934105 ) ) ;
#11695 = CARTESIAN_POINT ( 'NONE',  ( -1.500000000000000888, 6.245698675651501825E-16, 5.100000000000000533 ) ) ;
#11696 = ORIENTED_EDGE ( 'NONE', *, *, #5408, .F. ) ;
#11697 = FACE_OUTER_BOUND ( 'NONE', #4014, .T. ) ;
#11698 = EDGE_LOOP ( 'NONE', ( #3944, #2123 ) ) ;
#11699 = CARTESIAN_POINT ( 'NONE',  ( 0.000000000000000000, -0.6000000000000000888, 2.622672778259560467 ) ) ;
#11700 =( NAMED_UNIT ( * ) PLANE_ANGLE_UNIT ( ) SI_UNIT ( $, .RADIAN. ) );
#11701 = DIRECTION ( 'NONE',  ( -0.000000000000000000, 1.000000000000000000, -0.000000000000000000 ) ) ;
#11702 = DIRECTION ( 'NONE',  ( 0.000000000000000000, 0.000000000000000000, 1.000000000000000000 ) ) ;
#11703 = LINE ( 'NONE', #2390, #9850 ) ;
#11704 = ORIENTED_EDGE ( 'NONE', *, *, #11830, .F. ) ;
#11705 = VERTEX_POINT ( 'NONE', #10136 ) ;
#11706 = DIRECTION ( 'NONE',  ( 0.000000000000000000, -1.000000000000000000, 0.000000000000000000 ) ) ;
#11707 = ORIENTED_EDGE ( 'NONE', *, *, #283, .F. ) ;
#11708 = ADVANCED_FACE ( 'NONE', ( #5631 ), #3634, .T. ) ;
#11709 = EDGE_CURVE ( 'NONE', #1937, #7142, #1237, .T. ) ;
#11710 = DIRECTION ( 'NONE',  ( 0.000000000000000000, -0.4999999999999993894, 0.8660254037844389297 ) ) ;
#11711 = EDGE_LOOP ( 'NONE', ( #8314, #4537, #4134, #11334 ) ) ;
#11712 = CYLINDRICAL_SURFACE ( 'NONE', #9193, 9.600000000009600853 ) ;
#11713 = CARTESIAN_POINT ( 'NONE',  ( 0.000000000000000000, 0.000000000000000000, 0.000000000000000000 ) ) ;
#11714 = DIRECTION ( 'NONE',  ( -1.000000000000000000, 0.000000000000000000, -0.000000000000000000 ) ) ;
#11715 = DIRECTION ( 'NONE',  ( 0.000000000000000000, 0.000000000000000000, 1.000000000000000000 ) ) ;
#11716 = ORIENTED_EDGE ( 'NONE', *, *, #7478, .T. ) ;
#11717 = ORIENTED_EDGE ( 'NONE', *, *, #9786, .T. ) ;
#11718 = SURFACE_STYLE_FILL_AREA ( #11784 ) ;
#11719 = ORIENTED_EDGE ( 'NONE', *, *, #9635, .T. ) ;
#11720 = CARTESIAN_POINT ( 'NONE',  ( 0.000000000000000000, -14.40062958310459251, -8.872489362018340486 ) ) ;
#11721 = EDGE_CURVE ( 'NONE', #661, #1926, #879, .T. ) ;
#11722 = DIRECTION ( 'NONE',  ( 0.000000000000000000, 0.7071067811865486830, -0.7071067811865464625 ) ) ;
#11723 = EDGE_CURVE ( 'NONE', #7555, #4240, #7234, .T. ) ;
#11724 = EDGE_CURVE ( 'NONE', #7793, #8701, #8833, .T. ) ;
#11725 = EDGE_CURVE ( 'NONE', #1709, #1424, #1840, .T. ) ;
#11726 = CARTESIAN_POINT ( 'NONE',  ( 0.5590169943749477843, 0.000000000000000000, 0.000000000000000000 ) ) ;
#11727 = ORIENTED_EDGE ( 'NONE', *, *, #2399, .T. ) ;
#11728 = DIRECTION ( 'NONE',  ( 1.000000000000000000, -0.000000000000000000, -0.000000000000000000 ) ) ;
#11729 = CARTESIAN_POINT ( 'NONE',  ( 0.000000000000000000, 17.79862902732283914, -13.85025647830039119 ) ) ;
#11730 = ORIENTED_EDGE ( 'NONE', *, *, #7533, .F. ) ;
#11731 = CYLINDRICAL_SURFACE ( 'NONE', #4259, 7.200000000007202416 ) ;
#11732 = SHAPE_REPRESENTATION_RELATIONSHIP ( 'NONE' , 'NONE' ,  #8426, #4358 ) ;
#11733 = CYLINDRICAL_SURFACE ( 'NONE', #10427, 25.00000000000000000 ) ;
#11734 = DIRECTION ( 'NONE',  ( 0.000000000000000000, -1.000000000000000000, 0.000000000000000000 ) ) ;
#11735 = EDGE_CURVE ( 'NONE', #11705, #4464, #7637, .T. ) ;
#11736 = ORIENTED_EDGE ( 'NONE', *, *, #2208, .T. ) ;
#11737 = CARTESIAN_POINT ( 'NONE',  ( 25.00000000000000000, 0.000000000000000000, 5.000000000000000000 ) ) ;
#11738 = AXIS2_PLACEMENT_3D ( 'NONE', #7749, #2737, #8629 ) ;
#11739 = AXIS2_PLACEMENT_3D ( 'NONE', #9268, #11178, #6448 ) ;
#11740 = CARTESIAN_POINT ( 'NONE',  ( 0.000000000000000000, 0.000000000000000000, 7.000000000000000000 ) ) ;
#11741 = DIRECTION ( 'NONE',  ( 1.000000000000000000, -0.000000000000000000, -0.000000000000000000 ) ) ;
#11742 = LINE ( 'NONE', #7081, #6407 ) ;
#11743 = DIRECTION ( 'NONE',  ( 0.000000000000000000, 0.000000000000000000, -1.000000000000000000 ) ) ;
#11744 = DIRECTION ( 'NONE',  ( 1.000000000000000000, 0.000000000000000000, -0.000000000000000000 ) ) ;
#11745 = VERTEX_POINT ( 'NONE', #7708 ) ;
#11746 = VERTEX_POINT ( 'NONE', #72 ) ;
#11747 = FACE_OUTER_BOUND ( 'NONE', #6649, .T. ) ;
#11748 = DIRECTION ( 'NONE',  ( -1.000000000000000000, -3.903127820947815962E-18, 0.000000000000000000 ) ) ;
#11749 = AXIS2_PLACEMENT_3D ( 'NONE', #6306, #11049, #11853 ) ;
#11750 = VERTEX_POINT ( 'NONE', #183 ) ;
#11751 = DIRECTION ( 'NONE',  ( 1.000000000000000000, 0.000000000000000000, 0.000000000000000000 ) ) ;
#11752 = APPLICATION_CONTEXT ( 'automotive_design' ) ;
#11753 = VECTOR ( 'NONE', #4274, 1000.000000000000000 ) ;
#11754 = ADVANCED_FACE ( 'NONE', ( #3997 ), #10696, .F. ) ;
#11755 = VERTEX_POINT ( 'NONE', #126 ) ;
#11756 = DIRECTION ( 'NONE',  ( 1.000000000000000000, -0.000000000000000000, -0.000000000000000000 ) ) ;
#11757 = AXIS2_PLACEMENT_3D ( 'NONE', #11091, #9346, #8228 ) ;
#11758 = VECTOR ( 'NONE', #10706, 1000.000000000000000 ) ;
#11759 = DIRECTION ( 'NONE',  ( -1.000000000000000000, 0.000000000000000000, 0.000000000000000000 ) ) ;
#11760 = CARTESIAN_POINT ( 'NONE',  ( 4.999999999999997335, 6.799999999999999822, 1.500000000000000000 ) ) ;
#11761 = AXIS2_PLACEMENT_3D ( 'NONE', #11688, #10699, #254 ) ;
#11762 = VECTOR ( 'NONE', #8014, 1000.000000000000000 ) ;
#11763 = DIRECTION ( 'NONE',  ( 0.000000000000000000, 0.5068368027542901055, -0.8620420264545163302 ) ) ;
#11764 = DIRECTION ( 'NONE',  ( -1.000000000000000000, 0.000000000000000000, 0.000000000000000000 ) ) ;
#11765 = ORIENTED_EDGE ( 'NONE', *, *, #5315, .F. ) ;
#11766 = ORIENTED_EDGE ( 'NONE', *, *, #8239, .F. ) ;
#11767 = CARTESIAN_POINT ( 'NONE',  ( 0.000000000000000000, -19.60720892790245529, -11.14352537685195266 ) ) ;
#11768 = ITEM_DEFINED_TRANSFORMATION ( 'NONE', 'NONE', #61,  #6056 ) ;
#11769 = ORIENTED_EDGE ( 'NONE', *, *, #8089, .T. ) ;
#11770 = AXIS2_PLACEMENT_3D ( 'NONE', #7365, #7434, #11105 ) ;
#11771 = CARTESIAN_POINT ( 'NONE',  ( 4.999999999999999112, -5.955107813822691831, 26.33508479058318485 ) ) ;
#11772 = DIRECTION ( 'NONE',  ( -1.000000000000000000, 0.000000000000000000, 0.000000000000000000 ) ) ;
#11773 = CARTESIAN_POINT ( 'NONE',  ( 2.500000000000000000, -2.357898499370432610, 3.252606517456513302E-15 ) ) ;
#11774 = DIRECTION ( 'NONE',  ( 0.000000000000000000, 0.000000000000000000, 1.000000000000000000 ) ) ;
#11775 = CARTESIAN_POINT ( 'NONE',  ( 4.999999999999999112, 0.000000000000000000, 0.000000000000000000 ) ) ;
#11776 = CIRCLE ( 'NONE', #1604, 7.200000000007204193 ) ;
#11777 = EDGE_CURVE ( 'NONE', #5455, #2990, #9439, .T. ) ;
#11778 = EDGE_LOOP ( 'NONE', ( #8889, #8173, #10327, #9888 ) ) ;
#11779 = VECTOR ( 'NONE', #8900, 1000.000000000000000 ) ;
#11780 = CARTESIAN_POINT ( 'NONE',  ( 2.500000000000000000, 0.000000000000000000, 0.000000000000000000 ) ) ;
#11781 = TOROIDAL_SURFACE ( 'NONE', #796, 7.399999999999999467, 0.1000000000000000472 ) ;
#11782 = ORIENTED_EDGE ( 'NONE', *, *, #5003, .T. ) ;
#11783 = EDGE_CURVE ( 'NONE', #9763, #1333, #1242, .T. ) ;
#11784 = FILL_AREA_STYLE ('',( #5931 ) ) ;
#11785 = EDGE_LOOP ( 'NONE', ( #269, #606, #3687, #4333, #9555 ) ) ;
#11786 = DIRECTION ( 'NONE',  ( 0.000000000000000000, 0.000000000000000000, 1.000000000000000000 ) ) ;
#11787 = DIRECTION ( 'NONE',  ( -1.000000000000000000, 0.000000000000000000, -0.000000000000000000 ) ) ;
#11788 = CIRCLE ( 'NONE', #3222, 5.999999999999999112 ) ;
#11789 = VECTOR ( 'NONE', #9350, 1000.000000000000000 ) ;
#11790 = AXIS2_PLACEMENT_3D ( 'NONE', #4606, #5603, #601 ) ;
#11791 = CARTESIAN_POINT ( 'NONE',  ( -10.00000000000000000, 44.00000000000001421, -12.50000000000000000 ) ) ;
#11792 = ADVANCED_FACE ( 'NONE', ( #2887 ), #2073, .F. ) ;
#11793 = ORIENTED_EDGE ( 'NONE', *, *, #6309, .T. ) ;
#11795 = DIRECTION ( 'NONE',  ( -0.000000000000000000, -0.000000000000000000, -1.000000000000000000 ) ) ;
#11794 = COLOUR_RGB ( '',0.8941176470588234615, 0.8941176470588234615, 0.8941176470588234615 ) ;
#11796 = VECTOR ( 'NONE', #11916, 1000.000000000000000 ) ;
#11797 = VERTEX_POINT ( 'NONE', #2813 ) ;
#11798 = AXIS2_PLACEMENT_3D ( 'NONE', #2646, #8404, #9402 ) ;
#11799 = DIRECTION ( 'NONE',  ( 1.000000000000000000, 0.000000000000000000, 0.000000000000000000 ) ) ;
#11800 = EDGE_CURVE ( 'NONE', #4422, #2927, #2126, .T. ) ;
#11801 = CIRCLE ( 'NONE', #6429, 7.200000000007200640 ) ;
#11802 = CARTESIAN_POINT ( 'NONE',  ( 4.999999999999999112, 0.000000000000000000, 0.000000000000000000 ) ) ;
#11803 = VECTOR ( 'NONE', #6240, 1000.000000000000000 ) ;
#11804 = ADVANCED_FACE ( 'NONE', ( #3081 ), #9759, .F. ) ;
#11805 = DIRECTION ( 'NONE',  ( -1.000000000000000000, -0.000000000000000000, -0.000000000000000000 ) ) ;
#11806 = EDGE_LOOP ( 'NONE', ( #1232, #12072, #3468, #10335, #2479, #9476, #9938, #3398, #9624, #8805 ) ) ;
#11807 = DIRECTION ( 'NONE',  ( 0.000000000000000000, 1.224646799147353207E-16, 1.000000000000000000 ) ) ;
#11808 = AXIS2_PLACEMENT_3D ( 'NONE', #8666, #7859, #8596 ) ;
#11809 = AXIS2_PLACEMENT_3D ( 'NONE', #376, #4260, #10761 ) ;
#11810 = CIRCLE ( 'NONE', #2635, 7.200000000007200640 ) ;
#11811 = CARTESIAN_POINT ( 'NONE',  ( 36.00000000000000711, 0.000000000000000000, 0.000000000000000000 ) ) ;
#11812 = CARTESIAN_POINT ( 'NONE',  ( 4.999999999999999112, 0.000000000000000000, 0.000000000000000000 ) ) ;
#11813 = CARTESIAN_POINT ( 'NONE',  ( 15.00000000000000355, 44.00000000000001421, 2.149999999999999023 ) ) ;
#11814 = LINE ( 'NONE', #11872, #9859 ) ;
#11815 = EDGE_LOOP ( 'NONE', ( #2211, #4480, #11342, #7330 ) ) ;
#11816 = ORIENTED_EDGE ( 'NONE', *, *, #1130, .F. ) ;
#11817 = DIRECTION ( 'NONE',  ( 0.000000000000000000, 0.7071067811865437980, 0.7071067811865512365 ) ) ;
#11818 = CARTESIAN_POINT ( 'NONE',  ( 0.000000000000000000, 4.769696007084728073, -1.500000000000000000 ) ) ;
#11819 = PRODUCT_DEFINITION_FORMATION_WITH_SPECIFIED_SOURCE ( 'ANY', '', #132, .NOT_KNOWN. ) ;
#11820 = CIRCLE ( 'NONE', #12219, 9.600000000009600853 ) ;
#11821 = ORIENTED_EDGE ( 'NONE', *, *, #8938, .T. ) ;
#11822 = FACE_OUTER_BOUND ( 'NONE', #27, .T. ) ;
#11823 = CIRCLE ( 'NONE', #12205, 2.000000000000000000 ) ;
#11824 = CIRCLE ( 'NONE', #7261, 7.200000000007202416 ) ;
#11825 = ORIENTED_EDGE ( 'NONE', *, *, #9622, .T. ) ;
#11826 = DIRECTION ( 'NONE',  ( 0.000000000000000000, 0.000000000000000000, 1.000000000000000000 ) ) ;
#11827 = CIRCLE ( 'NONE', #1254, 9.600000000009600853 ) ;
#11828 = DIRECTION ( 'NONE',  ( 1.000000000000000000, 0.000000000000000000, 0.000000000000000000 ) ) ;
#11829 = DIRECTION ( 'NONE',  ( 1.000000000000000000, -0.000000000000000000, -0.000000000000000000 ) ) ;
#11830 = EDGE_CURVE ( 'NONE', #12260, #681, #10503, .T. ) ;
#11831 = AXIS2_PLACEMENT_3D ( 'NONE', #11308, #2810, #7571 ) ;
#11832 = ORIENTED_EDGE ( 'NONE', *, *, #11295, .F. ) ;
#11833 = EDGE_CURVE ( 'NONE', #3968, #3546, #8847, .T. ) ;
#11834 = CARTESIAN_POINT ( 'NONE',  ( 4.999999999999999112, -14.88411597386723351, -8.035066368449358620 ) ) ;
#11835 = CARTESIAN_POINT ( 'NONE',  ( -10.00000000000000000, 0.000000000000000000, 0.000000000000000000 ) ) ;
#11836 = ORIENTED_EDGE ( 'NONE', *, *, #4055, .F. ) ;
#11837 = DIRECTION ( 'NONE',  ( 0.000000000000000000, 0.000000000000000000, -1.000000000000000000 ) ) ;
#11838 = VERTEX_POINT ( 'NONE', #5696 ) ;
#11839 = DIRECTION ( 'NONE',  ( 1.000000000000000000, 0.000000000000000000, 0.000000000000000000 ) ) ;
#11840 = ORIENTED_EDGE ( 'NONE', *, *, #10670, .F. ) ;
#11841 = VECTOR ( 'NONE', #5746, 1000.000000000000000 ) ;
#11842 = CARTESIAN_POINT ( 'NONE',  ( 4.999999999999999112, 19.60720892790252989, 11.14352537685181588 ) ) ;
#11843 = DIRECTION ( 'NONE',  ( 0.000000000000000000, 0.000000000000000000, 1.000000000000000000 ) ) ;
#11844 = CARTESIAN_POINT ( 'NONE',  ( 4.999999999999999112, -13.17168466712917585, -15.37949036966225513 ) ) ;
#11845 = CARTESIAN_POINT ( 'NONE',  ( -2.595115354961444076, -7.673029147243174641, -1.000000000000000000 ) ) ;
#11846 = DIRECTION ( 'NONE',  ( 0.000000000000000000, 0.000000000000000000, -1.000000000000000000 ) ) ;
#11847 = ORIENTED_EDGE ( 'NONE', *, *, #9434, .T. ) ;
#11848 = AXIS2_PLACEMENT_3D ( 'NONE', #8287, #5472, #577 ) ;
#11849 = DIRECTION ( 'NONE',  ( 0.000000000000000000, -0.7091011189803928527, 0.7051068025914618564 ) ) ;
#11850 = VERTEX_POINT ( 'NONE', #12303 ) ;
#11851 = ORIENTED_EDGE ( 'NONE', *, *, #4021, .F. ) ;
#11852 = CARTESIAN_POINT ( 'NONE',  ( -1.500000000000001332, 0.000000000000000000, 0.000000000000000000 ) ) ;
#11853 = DIRECTION ( 'NONE',  ( 0.000000000000000000, 0.000000000000000000, 1.000000000000000000 ) ) ;
#11854 = AXIS2_PLACEMENT_3D ( 'NONE', #4585, #8406, #12197 ) ;
#11855 = CARTESIAN_POINT ( 'NONE',  ( 36.00000000000000000, 40.00000000000000711, 20.00000000000001066 ) ) ;
#11856 = EDGE_CURVE ( 'NONE', #1686, #2298, #11022, .T. ) ;
#11857 = ORIENTED_EDGE ( 'NONE', *, *, #2651, .F. ) ;
#11858 = CYLINDRICAL_SURFACE ( 'NONE', #1788, 7.000000000000000000 ) ;
#11859 = ORIENTED_EDGE ( 'NONE', *, *, #9835, .F. ) ;
#11860 = CARTESIAN_POINT ( 'NONE',  ( 46.00000000000000000, 6.123233995736773185E-16, -46.99999999999999289 ) ) ;
#11861 = CARTESIAN_POINT ( 'NONE',  ( -10.00000000000000000, 0.000000000000000000, 0.000000000000000000 ) ) ;
#11862 = ORIENTED_EDGE ( 'NONE', *, *, #11211, .T. ) ;
#11863 = CARTESIAN_POINT ( 'NONE',  ( 2.500000000000000000, 2.357898499370433054, -1.951563910473907981E-15 ) ) ;
#11864 = EDGE_CURVE ( 'NONE', #5923, #9911, #11548, .T. ) ;
#11865 = DIRECTION ( 'NONE',  ( 1.000000000000000000, 0.000000000000000000, 0.000000000000000000 ) ) ;
#11866 = EDGE_CURVE ( 'NONE', #11929, #8025, #5843, .T. ) ;
#11867 = VECTOR ( 'NONE', #10638, 1000.000000000000000 ) ;
#11868 = ADVANCED_FACE ( 'NONE', ( #11495 ), #2940, .T. ) ;
#11869 = FACE_OUTER_BOUND ( 'NONE', #2599, .T. ) ;
#11870 = CARTESIAN_POINT ( 'NONE',  ( 4.999999999999999112, -14.40062958310459251, -8.872489362018340486 ) ) ;
#11871 = LINE ( 'NONE', #371, #8064 ) ;
#11872 = CARTESIAN_POINT ( 'NONE',  ( 0.000000000000000000, -2.357898499370432610, 3.252606517456513302E-15 ) ) ;
#11873 = ORIENTED_EDGE ( 'NONE', *, *, #7910, .F. ) ;
#11874 = ORIENTED_EDGE ( 'NONE', *, *, #449, .T. ) ;
#11875 = DIRECTION ( 'NONE',  ( 0.000000000000000000, 0.000000000000000000, -1.000000000000000000 ) ) ;
#11876 = DIRECTION ( 'NONE',  ( -2.731402571913187487E-17, -0.5883347247165658933, 0.8086174940555531654 ) ) ;
#11877 = ORIENTED_EDGE ( 'NONE', *, *, #2284, .T. ) ;
#11878 = DIRECTION ( 'NONE',  ( 1.000000000000000000, 0.000000000000000000, 0.000000000000000000 ) ) ;
#11879 = ORIENTED_EDGE ( 'NONE', *, *, #3181, .T. ) ;
#11880 = DIRECTION ( 'NONE',  ( 0.000000000000000000, 0.000000000000000000, -1.000000000000000000 ) ) ;
#11881 = EDGE_CURVE ( 'NONE', #6450, #10109, #436, .T. ) ;
#11882 = ADVANCED_FACE ( 'NONE', ( #3002 ), #11733, .T. ) ;
#11883 = EDGE_CURVE ( 'NONE', #4951, #11004, #2303, .T. ) ;
#11884 = CARTESIAN_POINT ( 'NONE',  ( 2.499999999999999556, 5.955107813822860585, -26.33508479058314933 ) ) ;
#11885 = LINE ( 'NONE', #2206, #172 ) ;
#11886 = DIRECTION ( 'NONE',  ( -1.000000000000000000, 0.000000000000000000, 0.000000000000000000 ) ) ;
#11887 = DIRECTION ( 'NONE',  ( -1.000000000000000000, -0.000000000000000000, -0.000000000000000000 ) ) ;
#11888 = ORIENTED_EDGE ( 'NONE', *, *, #3810, .F. ) ;
#11889 = DIRECTION ( 'NONE',  ( 0.000000000000000000, -0.5446390350150290827, 0.8386705679454227180 ) ) ;
#11890 = ORIENTED_EDGE ( 'NONE', *, *, #3900, .T. ) ;
#11891 = CARTESIAN_POINT ( 'NONE',  ( 2.500000000000000000, 2.357898499370433054, -1.951563910473907981E-15 ) ) ;
#11892 = ORIENTED_EDGE ( 'NONE', *, *, #2207, .F. ) ;
#11893 = EDGE_CURVE ( 'NONE', #11679, #7959, #2358, .T. ) ;
#11894 = EDGE_CURVE ( 'NONE', #11589, #6154, #251, .T. ) ;
#11895 = CARTESIAN_POINT ( 'NONE',  ( 2.500000000000000000, 1.178949249685213863, -2.042000000000001148 ) ) ;
#11896 = DIRECTION ( 'NONE',  ( -1.000000000000000000, 0.000000000000000000, 0.000000000000000000 ) ) ;
#11897 = CARTESIAN_POINT ( 'NONE',  ( 3.309651814758564736, -5.455921364805393026, -1.000000000000000000 ) ) ;
#11898 = CARTESIAN_POINT ( 'NONE',  ( 50.00005079999999680, 0.000000000000000000, 0.000000000000000000 ) ) ;
#11899 = DIRECTION ( 'NONE',  ( 0.000000000000000000, 0.000000000000000000, 1.000000000000000000 ) ) ;
#11900 = ORIENTED_EDGE ( 'NONE', *, *, #10613, .F. ) ;
#11901 = FACE_OUTER_BOUND ( 'NONE', #2874, .T. ) ;
#11902 = VERTEX_POINT ( 'NONE', #3190 ) ;
#11903 = EDGE_LOOP ( 'NONE', ( #5434, #8948, #8141, #9186, #1103, #5738, #9275, #8821, #5312, #11969, #8299, #12312, #4778, #8065, #10145, #545 ) ) ;
#11904 = DIRECTION ( 'NONE',  ( 1.000000000000000000, 0.000000000000000000, 0.000000000000000000 ) ) ;
#11905 = EDGE_CURVE ( 'NONE', #9112, #1937, #7653, .T. ) ;
#11906 = CARTESIAN_POINT ( 'NONE',  ( 65.79898987322334847, -5.000000000000004441, -41.99999999999998579 ) ) ;
#11907 = VERTEX_POINT ( 'NONE', #11860 ) ;
#11908 = DIRECTION ( 'NONE',  ( 0.000000000000000000, -1.000000000000000000, -1.036015409262890124E-14 ) ) ;
#11909 = ORIENTED_EDGE ( 'NONE', *, *, #6760, .F. ) ;
#11910 = CARTESIAN_POINT ( 'NONE',  ( 33.00000000000000000, 0.000000000000000000, -41.99999999999999289 ) ) ;
#11911 = ORIENTED_EDGE ( 'NONE', *, *, #7647, .T. ) ;
#11912 = DIRECTION ( 'NONE',  ( 0.000000000000000000, 0.000000000000000000, 1.000000000000000000 ) ) ;
#11913 = VERTEX_POINT ( 'NONE', #10874 ) ;
#11914 = DIRECTION ( 'NONE',  ( 0.000000000000000000, 0.000000000000000000, -1.000000000000000000 ) ) ;
#11915 = FACE_OUTER_BOUND ( 'NONE', #10909, .T. ) ;
#11916 = DIRECTION ( 'NONE',  ( -1.000000000000000000, 0.000000000000000000, -0.000000000000000000 ) ) ;
#11917 = DIRECTION ( 'NONE',  ( -1.000000000000000000, 0.000000000000000000, -0.000000000000000000 ) ) ;
#11918 = CARTESIAN_POINT ( 'NONE',  ( 4.999999999999999112, 0.000000000000000000, 0.000000000000000000 ) ) ;
#11919 = CARTESIAN_POINT ( 'NONE',  ( 37.00000000000000711, -2.263420294706660396, 4.458354917400590978 ) ) ;
#11920 = ORIENTED_EDGE ( 'NONE', *, *, #5934, .F. ) ;
#11921 = ORIENTED_EDGE ( 'NONE', *, *, #12328, .T. ) ;
#11922 = EDGE_CURVE ( 'NONE', #4422, #4040, #2843, .T. ) ;
#11923 = CARTESIAN_POINT ( 'NONE',  ( 29.00000000000000000, 0.000000000000000000, -41.99999999999999289 ) ) ;
#11924 = PRESENTATION_STYLE_ASSIGNMENT (( #11125 ) ) ;
#11925 = DIRECTION ( 'NONE',  ( 0.000000000000000000, 0.8772744497699203059, 0.4799891038147465760 ) ) ;
#11926 = VERTEX_POINT ( 'NONE', #5251 ) ;
#11927 = FACE_OUTER_BOUND ( 'NONE', #3738, .T. ) ;
#11928 = ADVANCED_FACE ( 'NONE', ( #1181 ), #243, .F. ) ;
#11929 = VERTEX_POINT ( 'NONE', #10810 ) ;
#11930 = LINE ( 'NONE', #8391, #3041 ) ;
#11931 = VECTOR ( 'NONE', #3545, 1000.000000000000000 ) ;
#11932 = AXIS2_PLACEMENT_3D ( 'NONE', #5377, #4558, #11247 ) ;
#11933 = VECTOR ( 'NONE', #3577, 1000.000000000000000 ) ;
#11934 = ORIENTED_EDGE ( 'NONE', *, *, #11550, .T. ) ;
#11935 = DIRECTION ( 'NONE',  ( 0.000000000000000000, 0.000000000000000000, 1.000000000000000000 ) ) ;
#11936 = DIRECTION ( 'NONE',  ( -1.000000000000000000, -0.000000000000000000, 0.000000000000000000 ) ) ;
#11937 = CARTESIAN_POINT ( 'NONE',  ( 0.2500000000000002220, 0.000000000000000000, 0.000000000000000000 ) ) ;
#11938 = DIRECTION ( 'NONE',  ( -1.000000000000000000, -0.000000000000000000, -0.000000000000000000 ) ) ;
#11939 = AXIS2_PLACEMENT_3D ( 'NONE', #11103, #9310, #9252 ) ;
#11940 = CIRCLE ( 'NONE', #6178, 9.600000000009600853 ) ;
#11941 = EDGE_LOOP ( 'NONE', ( #10257, #6465, #5383, #8745 ) ) ;
#11942 = EDGE_CURVE ( 'NONE', #8024, #3084, #10628, .T. ) ;
#11943 = DIRECTION ( 'NONE',  ( -1.000000000000000000, 4.770489558936235687E-18, -6.855277276495154548E-34 ) ) ;
#11944 = CARTESIAN_POINT ( 'NONE',  ( 4.999999999999999112, 13.17168466712950092, -15.37949036966198157 ) ) ;
#11945 = VERTEX_POINT ( 'NONE', #9939 ) ;
#11946 = CARTESIAN_POINT ( 'NONE',  ( 4.999999999999999112, -13.85025647830069317, 17.79862902732260110 ) ) ;
#11947 = EDGE_CURVE ( 'NONE', #7499, #2623, #9849, .T. ) ;
#11948 = EDGE_CURVE ( 'NONE', #720, #11478, #9044, .T. ) ;
#11949 = ORIENTED_EDGE ( 'NONE', *, *, #9376, .F. ) ;
#11950 = ADVANCED_FACE ( 'NONE', ( #4245 ), #1359, .T. ) ;
#11951 = AXIS2_PLACEMENT_3D ( 'NONE', #9472, #2952, #893 ) ;
#11952 = AXIS2_PLACEMENT_3D ( 'NONE', #4640, #8459, #11807 ) ;
#11953 = DIRECTION ( 'NONE',  ( -1.000000000000000000, -0.000000000000000000, -0.000000000000000000 ) ) ;
#11954 = MECHANICAL_DESIGN_GEOMETRIC_PRESENTATION_REPRESENTATION (  '', ( #5777 ), #11362 ) ;
#11955 = DIRECTION ( 'NONE',  ( -0.9995235871707960351, -0.03086419753086420970, 0.000000000000000000 ) ) ;
#11956 = DIRECTION ( 'NONE',  ( -1.000000000000000000, 0.000000000000000000, -0.000000000000000000 ) ) ;
#11957 = CARTESIAN_POINT ( 'NONE',  ( 0.000000000000000000, 0.000000000000000000, 0.000000000000000000 ) ) ;
#11958 = LINE ( 'NONE', #3349, #6015 ) ;
#11959 = ORIENTED_EDGE ( 'NONE', *, *, #8998, .F. ) ;
#11960 = CARTESIAN_POINT ( 'NONE',  ( 4.999999999999999112, -20.13931372320393010, 5.950465759858794002 ) ) ;
#11961 = ORIENTED_EDGE ( 'NONE', *, *, #10762, .F. ) ;
#11962 = DIRECTION ( 'NONE',  ( 1.000000000000000000, 0.000000000000000000, 0.000000000000000000 ) ) ;
#11963 = EDGE_LOOP ( 'NONE', ( #8152, #4735, #6931, #9443 ) ) ;
#11964 = COLOUR_RGB ( '',0.8941176470588234615, 0.8941176470588234615, 0.8941176470588234615 ) ;
#11965 = ADVANCED_FACE ( 'NONE', ( #4177 ), #8004, .T. ) ;
#11966 = CYLINDRICAL_SURFACE ( 'NONE', #6430, 27.00000000002699707 ) ;
#11967 = DIRECTION ( 'NONE',  ( 1.000000000000000000, 0.000000000000000000, 0.000000000000000000 ) ) ;
#11968=STYLED_ITEM('',(#12391),#8661);
#11969 = ORIENTED_EDGE ( 'NONE', *, *, #11584, .T. ) ;
#11970 = CARTESIAN_POINT ( 'NONE',  ( 24.00000000000000000, 0.000000000000000000, -41.99999999999999289 ) ) ;
#11971 = CIRCLE ( 'NONE', #6641, 5.000000000000000000 ) ;
#11972 = VECTOR ( 'NONE', #4929, 1000.000000000000000 ) ;
#11973 = ORIENTED_EDGE ( 'NONE', *, *, #5632, .T. ) ;
#11974 = EDGE_CURVE ( 'NONE', #10042, #6125, #53, .T. ) ;
#11975 = EDGE_CURVE ( 'NONE', #8289, #5929, #1248, .T. ) ;
#11976 = CARTESIAN_POINT ( 'NONE',  ( -3.309651814758565180, -5.455921364805393026, -1.000000000000000000 ) ) ;
#11977 = ORIENTED_EDGE ( 'NONE', *, *, #1680, .F. ) ;
#11978 = AXIS2_PLACEMENT_3D ( 'NONE', #5186, #4252, #10929 ) ;
#11979 = FACE_OUTER_BOUND ( 'NONE', #5781, .T. ) ;
#11980 = AXIS2_PLACEMENT_3D ( 'NONE', #4827, #8465, #9465 ) ;
#11981 = VERTEX_POINT ( 'NONE', #10108 ) ;
#11982 = DIRECTION ( 'NONE',  ( -1.000000000000000000, -0.000000000000000000, -0.000000000000000000 ) ) ;
#11983 = AXIS2_PLACEMENT_3D ( 'NONE', #2978, #5675, #6802 ) ;
#11984 = APPLICATION_CONTEXT ( 'automotive_design' ) ;
#11985 =( NAMED_UNIT ( * ) SI_UNIT ( $, .STERADIAN. ) SOLID_ANGLE_UNIT ( ) );
#11986 = VECTOR ( 'NONE', #7550, 1000.000000000000000 ) ;
#11987 = AXIS2_PLACEMENT_3D ( 'NONE', #2393, #10899, #11837 ) ;
#11988 = CARTESIAN_POINT ( 'NONE',  ( 0.2499999999999966416, -8.096141056083448362, -1.000000000000000000 ) ) ;
#11989 = DIRECTION ( 'NONE',  ( 0.000000000000000000, 0.000000000000000000, 1.000000000000000000 ) ) ;
#11990 = VECTOR ( 'NONE', #6690, 1000.000000000000000 ) ;
#11991 = VECTOR ( 'NONE', #7177, 1000.000000000000000 ) ;
#11992 = CARTESIAN_POINT ( 'NONE',  ( 0.000000000000000000, 13.09267581720874674, -5.622796541391427816 ) ) ;
#11993 = CARTESIAN_POINT ( 'NONE',  ( -33.00000000000000000, 0.000000000000000000, 0.000000000000000000 ) ) ;
#11994 = ORIENTED_EDGE ( 'NONE', *, *, #4779, .T. ) ;
#11995 = ORIENTED_EDGE ( 'NONE', *, *, #3596, .T. ) ;
#11996 = CARTESIAN_POINT ( 'NONE',  ( 17.00000000000000000, 0.000000000000000000, 2.055000000000000160 ) ) ;
#11997 = FILL_AREA_STYLE_COLOUR ( '', #9625 ) ;
#11998 = CARTESIAN_POINT ( 'NONE',  ( 1.500000000000001332, 0.000000000000000000, 0.000000000000000000 ) ) ;
#11999 = ORIENTED_EDGE ( 'NONE', *, *, #3023, .F. ) ;
#12000 = CARTESIAN_POINT ( 'NONE',  ( 33.00000000000000000, 0.000000000000000000, 6.500000000000000888 ) ) ;
#12001 = ORIENTED_EDGE ( 'NONE', *, *, #2889, .F. ) ;
#12002 = FACE_OUTER_BOUND ( 'NONE', #793, .T. ) ;
#12003 = CIRCLE ( 'NONE', #1235, 5.000000000000000000 ) ;
#12004 = AXIS2_PLACEMENT_3D ( 'NONE', #9330, #7279, #5512 ) ;
#12005 = AXIS2_PLACEMENT_3D ( 'NONE', #5915, #5717, #9536 ) ;
#12006 = VECTOR ( 'NONE', #698, 1000.000000000000000 ) ;
#12007 = CARTESIAN_POINT ( 'NONE',  ( 33.00000000000000000, 0.000000000000000000, -7.500000000000000888 ) ) ;
#12008 = DIRECTION ( 'NONE',  ( 1.387778780781445984E-17, 0.7900737791495477946, 0.6130117645692875206 ) ) ;
#12009 = EDGE_CURVE ( 'NONE', #3733, #3280, #1647, .T. ) ;
#12010 = FACE_BOUND ( 'NONE', #4113, .T. ) ;
#12011 = DIRECTION ( 'NONE',  ( -1.000000000000000000, 0.000000000000000000, 0.000000000000000000 ) ) ;
#12012 = AXIS2_PLACEMENT_3D ( 'NONE', #9569, #8641, #6709 ) ;
#12013 = PRODUCT_DEFINITION_SHAPE ( 'NONE', 'NONE',  #12368 ) ;
#12014 = EDGE_LOOP ( 'NONE', ( #7116, #11469, #4351, #10733, #5550 ) ) ;
#12015 = DIRECTION ( 'NONE',  ( 1.000000000000000000, -0.000000000000000000, -0.000000000000000000 ) ) ;
#12016 = AXIS2_PLACEMENT_3D ( 'NONE', #11835, #4272, #8862 ) ;
#12017 = CYLINDRICAL_SURFACE ( 'NONE', #3423, 4.000000000000003553 ) ;
#12018 = ORIENTED_EDGE ( 'NONE', *, *, #8830, .F. ) ;
#12019 =( NAMED_UNIT ( * ) SI_UNIT ( $, .STERADIAN. ) SOLID_ANGLE_UNIT ( ) );
#12020 = ORIENTED_EDGE ( 'NONE', *, *, #10800, .F. ) ;
#12021 = AXIS2_PLACEMENT_3D ( 'NONE', #6354, #10974, #10163 ) ;
#12022 = VECTOR ( 'NONE', #798, 1000.000000000000000 ) ;
#12023 = CIRCLE ( 'NONE', #8817, 20.24900000002025280 ) ;
#12024 = EDGE_CURVE ( 'NONE', #11497, #11670, #3351, .T. ) ;
#12025 = CIRCLE ( 'NONE', #8648, 9.600000000009602630 ) ;
#12026 = CARTESIAN_POINT ( 'NONE',  ( 0.000000000000000000, -26.60936692326687592, -4.576198416197529539 ) ) ;
#12027 = CYLINDRICAL_SURFACE ( 'NONE', #9982, 14.24900000001425227 ) ;
#12028 = CARTESIAN_POINT ( 'NONE',  ( -7.839872433920653082E-18, 0.000000000000000000, 0.000000000000000000 ) ) ;
#12029 = EDGE_CURVE ( 'NONE', #3834, #4584, #4225, .T. ) ;
#12030 = FACE_OUTER_BOUND ( 'NONE', #8216, .T. ) ;
#12032 = EDGE_CURVE ( 'NONE', #10334, #12260, #5229, .T. ) ;
#12031 = CARTESIAN_POINT ( 'NONE',  ( 4.999999999999999112, 0.000000000000000000, 0.000000000000000000 ) ) ;
#12033 = ORIENTED_EDGE ( 'NONE', *, *, #3699, .T. ) ;
#12034 = CARTESIAN_POINT ( 'NONE',  ( 4.999999999999999112, 0.000000000000000000, 0.000000000000000000 ) ) ;
#12035 = ORIENTED_EDGE ( 'NONE', *, *, #6071, .F. ) ;
#12036 =( NAMED_UNIT ( * ) SI_UNIT ( $, .STERADIAN. ) SOLID_ANGLE_UNIT ( ) );
#12037 = CARTESIAN_POINT ( 'NONE',  ( 34.50000000000000000, 1.364328772603918053E-31, -41.99999999999998579 ) ) ;
#12038 = AXIS2_PLACEMENT_3D ( 'NONE', #8891, #6997, #179 ) ;
#12039 = VERTEX_POINT ( 'NONE', #8063 ) ;
#12040 = DIRECTION ( 'NONE',  ( -1.000000000000000000, 0.000000000000000000, 0.000000000000000000 ) ) ;
#12041 = DIRECTION ( 'NONE',  ( -1.000000000000000000, -0.000000000000000000, -0.000000000000000000 ) ) ;
#12042 = VERTEX_POINT ( 'NONE', #11960 ) ;
#12043 = DIRECTION ( 'NONE',  ( 0.000000000000000000, 0.000000000000000000, 1.000000000000000000 ) ) ;
#12044 = EDGE_CURVE ( 'NONE', #10654, #3878, #6351, .T. ) ;
#12045 = ADVANCED_FACE ( 'NONE', ( #11901 ), #7244, .T. ) ;
#12046 = VERTEX_POINT ( 'NONE', #4342 ) ;
#12047 = CARTESIAN_POINT ( 'NONE',  ( 5.686050877451574337, -5.768780236673276995, -1.000000000000000000 ) ) ;
#12048 = EDGE_LOOP ( 'NONE', ( #7483, #4504, #286, #3709 ) ) ;
#12049 = CYLINDRICAL_SURFACE ( 'NONE', #5909, 21.00000000002100009 ) ;
#12050 = VECTOR ( 'NONE', #1152, 1000.000000000000000 ) ;
#12051 = ORIENTED_EDGE ( 'NONE', *, *, #8010, .T. ) ;
#12052 = DIRECTION ( 'NONE',  ( 0.000000000000000000, -0.9238795325112827417, -0.3826834323650997738 ) ) ;
#12053 = EDGE_CURVE ( 'NONE', #4049, #11745, #11823, .T. ) ;
#12054 = EDGE_CURVE ( 'NONE', #1455, #9068, #1442, .T. ) ;
#12055 = DIRECTION ( 'NONE',  ( 1.000000000000000000, 0.000000000000000000, 0.000000000000000000 ) ) ;
#12056 = FACE_OUTER_BOUND ( 'NONE', #1074, .T. ) ;
#12057 = AXIS2_PLACEMENT_3D ( 'NONE', #7722, #11387, #2761 ) ;
#12058 = DIRECTION ( 'NONE',  ( 0.000000000000000000, -1.000000000000000000, 0.000000000000000000 ) ) ;
#12059 = CARTESIAN_POINT ( 'NONE',  ( -0.1481481481481481122, -4.797713218419819903, 0.000000000000000000 ) ) ;
#12060 = EDGE_LOOP ( 'NONE', ( #5694, #9302, #1308, #6675 ) ) ;
#12061 = ORIENTED_EDGE ( 'NONE', *, *, #1273, .F. ) ;
#12062 = FACE_OUTER_BOUND ( 'NONE', #2856, .T. ) ;
#12063 = CARTESIAN_POINT ( 'NONE',  ( 51.00000000000000000, 0.000000000000000000, -44.50000000000000000 ) ) ;
#12064 = VERTEX_POINT ( 'NONE', #10910 ) ;
#12065 = CARTESIAN_POINT ( 'NONE',  ( -10.00000000000000000, 0.000000000000000000, 0.000000000000000000 ) ) ;
#12066 = VERTEX_POINT ( 'NONE', #11097 ) ;
#12067 = CARTESIAN_POINT ( 'NONE',  ( 17.00000000000000000, 2.055000000000000160, 0.000000000000000000 ) ) ;
#12068 = VECTOR ( 'NONE', #8574, 1000.000000000000000 ) ;
#12069 = CARTESIAN_POINT ( 'NONE',  ( 0.000000000000000000, 22.83261415639502800, 14.41081992069317508 ) ) ;
#12070 = FACE_OUTER_BOUND ( 'NONE', #3237, .T. ) ;
#12071 = CARTESIAN_POINT ( 'NONE',  ( 0.000000000000000000, 0.000000000000000000, 0.000000000000000000 ) ) ;
#12072 = ORIENTED_EDGE ( 'NONE', *, *, #4860, .T. ) ;
#12073 = CARTESIAN_POINT ( 'NONE',  ( -3.469446951953614189E-15, 66.91287847477919115, -12.50000000000000000 ) ) ;
#12074 = VECTOR ( 'NONE', #10300, 1000.000000000000000 ) ;
#12075 = DIRECTION ( 'NONE',  ( 1.000000000000000000, -0.000000000000000000, -0.000000000000000000 ) ) ;
#12076 = AXIS2_PLACEMENT_3D ( 'NONE', #9394, #8520, #5756 ) ;
#12077 = ORIENTED_EDGE ( 'NONE', *, *, #10286, .T. ) ;
#12078 = DIRECTION ( 'NONE',  ( 0.000000000000000000, 0.7900737791495477946, 0.6130117645692876316 ) ) ;
#12079 = ORIENTED_EDGE ( 'NONE', *, *, #9868, .T. ) ;
#12080 = PRESENTATION_STYLE_ASSIGNMENT (( #713 ) ) ;
#12081 = CARTESIAN_POINT ( 'NONE',  ( 43.00000000000000000, 3.903127820947864496E-18, 0.000000000000000000 ) ) ;
#12082 = PLANE ( 'NONE',  #4623 ) ;
#12083 = CARTESIAN_POINT ( 'NONE',  ( 51.00000000000000000, 3.500000000000001332, -45.49999999999998579 ) ) ;
#12084 = DIRECTION ( 'NONE',  ( 1.000000000000000000, 0.000000000000000000, 0.000000000000000000 ) ) ;
#12085 = PRODUCT ( 'handle', 'handle', '', ( #11407 ) ) ;
#12086 = ORIENTED_EDGE ( 'NONE', *, *, #6548, .T. ) ;
#12087 = CARTESIAN_POINT ( 'NONE',  ( 4.999999999999999112, 26.60936692326690434, -4.576198416197341245 ) ) ;
#12088 = VERTEX_POINT ( 'NONE', #9927 ) ;
#12089 = ADVANCED_FACE ( 'NONE', ( #1594 ), #3238, .T. ) ;
#12090 = DIRECTION ( 'NONE',  ( 1.000000000000000000, 0.000000000000000000, 0.000000000000000000 ) ) ;
#12091 = ORIENTED_EDGE ( 'NONE', *, *, #8939, .T. ) ;
#12092 = LINE ( 'NONE', #6117, #1035 ) ;
#12093 = EDGE_CURVE ( 'NONE', #9795, #6083, #405, .T. ) ;
#12094 = DIRECTION ( 'NONE',  ( 1.000000000000000000, 0.000000000000000000, 0.000000000000000000 ) ) ;
#12095 = ORIENTED_EDGE ( 'NONE', *, *, #6325, .T. ) ;
#12096 = DIRECTION ( 'NONE',  ( 0.000000000000000000, 0.000000000000000000, -1.000000000000000000 ) ) ;
#12097 = ORIENTED_EDGE ( 'NONE', *, *, #4302, .F. ) ;
#12098 = FACE_OUTER_BOUND ( 'NONE', #4387, .T. ) ;
#12099 = EDGE_LOOP ( 'NONE', ( #10384, #2160 ) ) ;
#12100 = EDGE_CURVE ( 'NONE', #10112, #11945, #10034, .T. ) ;
#12101 = DIRECTION ( 'NONE',  ( -1.000000000000000000, 0.000000000000000000, 0.000000000000000000 ) ) ;
#12102 = EDGE_CURVE ( 'NONE', #11745, #10319, #589, .T. ) ;
#12103 = ADVANCED_BREP_SHAPE_REPRESENTATION ( '', ( #4380, #6056 ), #6426 ) ;
#12105 = ORIENTED_EDGE ( 'NONE', *, *, #8361, .F. ) ;
#12104 = EDGE_CURVE ( 'NONE', #11586, #9428, #7855, .T. ) ;
#12106 = DIRECTION ( 'NONE',  ( 0.000000000000000000, -0.9238795325112826307, -0.3826834323650997183 ) ) ;
#12107 = ADVANCED_FACE ( 'NONE', ( #9119 ), #7984, .T. ) ;
#12108 = FACE_OUTER_BOUND ( 'NONE', #4861, .T. ) ;
#12109 = PLANE ( 'NONE',  #5454 ) ;
#12110 = DIRECTION ( 'NONE',  ( 0.000000000000000000, -1.000000000000000000, 0.000000000000000000 ) ) ;
#12111 = ORIENTED_EDGE ( 'NONE', *, *, #9960, .F. ) ;
#12112 = EDGE_LOOP ( 'NONE', ( #4543, #1611, #2643, #12211 ) ) ;
#12113 = CARTESIAN_POINT ( 'NONE',  ( 0.000000000000000000, -0.5999999999999996447, -2.622672778259560467 ) ) ;
#12114 = ADVANCED_FACE ( 'NONE', ( #4286 ), #7304, .T. ) ;
#12115 = CARTESIAN_POINT ( 'NONE',  ( 36.00000000000000711, -4.104405154062230115E-16, -2.224720805914714718E-17 ) ) ;
#12116 = ORIENTED_EDGE ( 'NONE', *, *, #12266, .T. ) ;
#12117 = DIRECTION ( 'NONE',  ( 0.000000000000000000, 0.000000000000000000, -1.000000000000000000 ) ) ;
#12118 = ORIENTED_EDGE ( 'NONE', *, *, #2816, .T. ) ;
#12119 = CARTESIAN_POINT ( 'NONE',  ( 36.00000000000000711, 1.456773409934505593E-31, -41.99999999999998579 ) ) ;
#12120 = FACE_OUTER_BOUND ( 'NONE', #9082, .T. ) ;
#12121 = DIRECTION ( 'NONE',  ( 1.000000000000000000, 0.000000000000000000, 0.000000000000000000 ) ) ;
#12122 = ORIENTED_EDGE ( 'NONE', *, *, #11477, .T. ) ;
#12123 = CARTESIAN_POINT ( 'NONE',  ( 4.999999999999997335, 0.000000000000000000, 0.000000000000000000 ) ) ;
#12124 = CARTESIAN_POINT ( 'NONE',  ( 46.00000000000000000, -3.499999999999998668, -38.49999999999998579 ) ) ;
#12125 = EDGE_LOOP ( 'NONE', ( #5867, #8932, #158, #4450, #8628, #11888 ) ) ;
#12126 = FACE_OUTER_BOUND ( 'NONE', #8807, .T. ) ;
#12127 = EDGE_CURVE ( 'NONE', #1723, #3694, #8172, .T. ) ;
#12128 = CARTESIAN_POINT ( 'NONE',  ( 5.000000000000000000, 0.000000000000000000, 1.500000000000000000 ) ) ;
#12129 = VECTOR ( 'NONE', #2296, 1000.000000000000000 ) ;
#12130 = ORIENTED_EDGE ( 'NONE', *, *, #9622, .F. ) ;
#12131 = FACE_OUTER_BOUND ( 'NONE', #8419, .T. ) ;
#12132 = EDGE_LOOP ( 'NONE', ( #6724, #2682, #2305, #1495 ) ) ;
#12133 = VECTOR ( 'NONE', #751, 1000.000000000000000 ) ;
#12134 = VECTOR ( 'NONE', #6660, 1000.000000000000000 ) ;
#12135 = LINE ( 'NONE', #12269, #9590 ) ;
#12136 = DIRECTION ( 'NONE',  ( 1.000000000000000000, 0.000000000000000000, -0.000000000000000000 ) ) ;
#12137 = VECTOR ( 'NONE', #3257, 1000.000000000000114 ) ;
#12138 = CARTESIAN_POINT ( 'NONE',  ( 0.000000000000000000, 0.000000000000000000, 0.000000000000000000 ) ) ;
#12139 = DIRECTION ( 'NONE',  ( 0.000000000000000000, 0.000000000000000000, -1.000000000000000000 ) ) ;
#12140 = ORIENTED_EDGE ( 'NONE', *, *, #3947, .F. ) ;
#12141 = ORIENTED_EDGE ( 'NONE', *, *, #5689, .F. ) ;
#12142 = CARTESIAN_POINT ( 'NONE',  ( 26.00000000000000355, 0.000000000000000000, -41.99999999999999289 ) ) ;
#12143 = ORIENTED_EDGE ( 'NONE', *, *, #7171, .T. ) ;
#12144 = SURFACE_STYLE_FILL_AREA ( #7069 ) ;
#12145 = CARTESIAN_POINT ( 'NONE',  ( -15.00000000000000000, 46.40000000000001279, 0.000000000000000000 ) ) ;
#12146 = VERTEX_POINT ( 'NONE', #8241 ) ;
#12148 = FACE_BOUND ( 'NONE', #7472, .T. ) ;
#12147 = VECTOR ( 'NONE', #5357, 1000.000000000000000 ) ;
#12149 = AXIS2_PLACEMENT_3D ( 'NONE', #7744, #2982, #6099 ) ;
#12150 = LINE ( 'NONE', #4603, #8774 ) ;
#12151 = CIRCLE ( 'NONE', #9787, 0.7500000000000000000 ) ;
#12152 = ORIENTED_EDGE ( 'NONE', *, *, #6701, .F. ) ;
#12153 = CARTESIAN_POINT ( 'NONE',  ( 37.00000000000000711, 0.000000000000000000, -1.500000000000000000 ) ) ;
#12154 = EDGE_CURVE ( 'NONE', #1937, #477, #11221, .T. ) ;
#12155 = AXIS2_PLACEMENT_3D ( 'NONE', #10460, #4762, #8586 ) ;
#12156 = CIRCLE ( 'NONE', #3383, 27.00000000002699707 ) ;
#12157 = EDGE_CURVE ( 'NONE', #1491, #6982, #12221, .T. ) ;
#12158 = ORIENTED_EDGE ( 'NONE', *, *, #4554, .T. ) ;
#12159 = DIRECTION ( 'NONE',  ( -0.000000000000000000, -1.000000000000000000, -0.000000000000000000 ) ) ;
#12160 = ORIENTED_EDGE ( 'NONE', *, *, #6091, .F. ) ;
#12161 =( LENGTH_UNIT ( ) NAMED_UNIT ( * ) SI_UNIT ( .MILLI., .METRE. ) );
#12162 = DIRECTION ( 'NONE',  ( -1.000000000000000000, 0.000000000000000000, 0.000000000000000000 ) ) ;
#12163 = ORIENTED_EDGE ( 'NONE', *, *, #396, .F. ) ;
#12164 = DIRECTION ( 'NONE',  ( -1.000000000000000000, -0.000000000000000000, 0.000000000000000000 ) ) ;
#12165 = CIRCLE ( 'NONE', #7591, 7.200000000007202416 ) ;
#12166 = VECTOR ( 'NONE', #3991, 1000.000000000000000 ) ;
#12167 = DIRECTION ( 'NONE',  ( -1.000000000000000000, -0.000000000000000000, 0.000000000000000000 ) ) ;
#12168 = EDGE_CURVE ( 'NONE', #866, #7442, #11395, .T. ) ;
#12169 = EDGE_CURVE ( 'NONE', #2396, #7170, #1457, .T. ) ;
#12170 = CARTESIAN_POINT ( 'NONE',  ( -10.00000000000000000, 0.000000000000000000, 0.000000000000000000 ) ) ;
#12171 = FACE_BOUND ( 'NONE', #3940, .T. ) ;
#12172 = EDGE_CURVE ( 'NONE', #2049, #10544, #6486, .T. ) ;
#12173 = AXIS2_PLACEMENT_3D ( 'NONE', #6912, #8720, #1146 ) ;
#12174 = ORIENTED_EDGE ( 'NONE', *, *, #4629, .T. ) ;
#12175 = EDGE_LOOP ( 'NONE', ( #1792, #1545, #7145, #553, #2262, #11637, #6587, #6544, #2350, #5920, #2138, #2410 ) ) ;
#12176 = CARTESIAN_POINT ( 'NONE',  ( -1.399999999999999689, 0.000000000000000000, -7.399999999999999467 ) ) ;
#12177 = AXIS2_PLACEMENT_3D ( 'NONE', #6715, #1079, #6577 ) ;
#12178 = CARTESIAN_POINT ( 'NONE',  ( 0.000000000000000000, 13.17168466712928598, 15.37949036966216632 ) ) ;
#12179 = TOROIDAL_SURFACE ( 'NONE', #6819, 5.100000000000000533, 0.1000000000000001582 ) ;
#12180 = CARTESIAN_POINT ( 'NONE',  ( 15.00000000000000355, 40.00000000000000711, 2.149999999999999023 ) ) ;
#12181 = ORIENTED_EDGE ( 'NONE', *, *, #822, .F. ) ;
#12182 = CYLINDRICAL_SURFACE ( 'NONE', #2840, 5.000000000000000000 ) ;
#12183 = EDGE_CURVE ( 'NONE', #6067, #3871, #12329, .T. ) ;
#12184 = VECTOR ( 'NONE', #5227, 1000.000000000000000 ) ;
#12185 = VECTOR ( 'NONE', #1478, 1000.000000000000000 ) ;
#12186 = SURFACE_STYLE_FILL_AREA ( #1641 ) ;
#12187 = DIRECTION ( 'NONE',  ( -1.000000000000000000, -0.000000000000000000, -0.000000000000000000 ) ) ;
#12188 = ORIENTED_EDGE ( 'NONE', *, *, #3476, .T. ) ;
#12189 = CARTESIAN_POINT ( 'NONE',  ( 4.999999999999999112, 22.37914155802285876, -2.791921004064323864 ) ) ;
#12190 = DIRECTION ( 'NONE',  ( -0.000000000000000000, -1.000000000000000000, -0.000000000000000000 ) ) ;
#12191 = ORIENTED_EDGE ( 'NONE', *, *, #4580, .T. ) ;
#12192 = DIRECTION ( 'NONE',  ( -1.000000000000000000, 0.000000000000000000, -0.000000000000000000 ) ) ;
#12193 = DIRECTION ( 'NONE',  ( 0.000000000000000000, 0.000000000000000000, 1.000000000000000000 ) ) ;
#12194 =( GEOMETRIC_REPRESENTATION_CONTEXT ( 3 ) GLOBAL_UNCERTAINTY_ASSIGNED_CONTEXT ( ( #10393 ) ) GLOBAL_UNIT_ASSIGNED_CONTEXT ( ( #8003, #7070, #3189 ) ) REPRESENTATION_CONTEXT ( 'NONE', 'WORKASPACE' ) );
#12195 = AXIS2_PLACEMENT_3D ( 'NONE', #8984, #9872, #5226 ) ;
#12196 = ORIENTED_EDGE ( 'NONE', *, *, #10971, .F. ) ;
#12197 = DIRECTION ( 'NONE',  ( 0.000000000000000000, 0.000000000000000000, 1.000000000000000000 ) ) ;
#12198 = AXIS2_PLACEMENT_3D ( 'NONE', #6381, #10189, #7513 ) ;
#12199 = VECTOR ( 'NONE', #4665, 1000.000000000000000 ) ;
#12200 = ORIENTED_EDGE ( 'NONE', *, *, #11505, .T. ) ;
#12201 = ADVANCED_FACE ( 'NONE', ( #10336 ), #4595, .T. ) ;
#12202 = SURFACE_STYLE_USAGE ( .BOTH. , #1024 ) ;
#12203 = EDGE_CURVE ( 'NONE', #7536, #3487, #8857, .T. ) ;
#12204 = CIRCLE ( 'NONE', #4834, 9.600000000009602630 ) ;
#12205 = AXIS2_PLACEMENT_3D ( 'NONE', #7115, #1535, #5351 ) ;
#12206 = DIRECTION ( 'NONE',  ( 0.000000000000000000, 0.000000000000000000, 1.000000000000000000 ) ) ;
#12207 = PLANE ( 'NONE',  #9019 ) ;
#12208 = VECTOR ( 'NONE', #5519, 1000.000000000000000 ) ;
#12209 = CARTESIAN_POINT ( 'NONE',  ( 0.2500000000000002220, 0.000000000000000000, 0.000000000000000000 ) ) ;
#12210 = CARTESIAN_POINT ( 'NONE',  ( 0.000000000000000000, 0.000000000000000000, 0.000000000000000000 ) ) ;
#12211 = ORIENTED_EDGE ( 'NONE', *, *, #4117, .T. ) ;
#12212 = ORIENTED_EDGE ( 'NONE', *, *, #8327, .F. ) ;
#12213 = DIRECTION ( 'NONE',  ( -1.000000000000000000, 0.000000000000000000, 0.000000000000000000 ) ) ;
#12214 = EDGE_LOOP ( 'NONE', ( #8348, #6812, #5759, #3485 ) ) ;
#12215 = DIRECTION ( 'NONE',  ( -1.000000000000000000, -0.000000000000000000, -0.000000000000000000 ) ) ;
#12216 = PRODUCT_CONTEXT ( 'NONE', #18, 'mechanical' ) ;
#12217 = ORIENTED_EDGE ( 'NONE', *, *, #6529, .T. ) ;
#12218 = ORIENTED_EDGE ( 'NONE', *, *, #11048, .F. ) ;
#12219 = AXIS2_PLACEMENT_3D ( 'NONE', #9041, #460, #6095 ) ;
#12220 = DIRECTION ( 'NONE',  ( 1.000000000000000000, -4.770489558936235687E-18, 6.855277276495153692E-34 ) ) ;
#12221 = CIRCLE ( 'NONE', #2821, 1.999999999999998224 ) ;
#12222 = AXIS2_PLACEMENT_3D ( 'NONE', #5903, #8023, #6019 ) ;
#12223 = CARTESIAN_POINT ( 'NONE',  ( 36.00000000000000711, -2.263420294706660396, 4.458354917400590978 ) ) ;
#12224 = EDGE_LOOP ( 'NONE', ( #10767, #3111, #11900, #9292 ) ) ;
#12225 = DIRECTION ( 'NONE',  ( 0.000000000000000000, 1.000000000000000000, -0.000000000000000000 ) ) ;
#12227 = DIRECTION ( 'NONE',  ( 0.000000000000000000, 0.000000000000000000, -1.000000000000000000 ) ) ;
#12226 = CIRCLE ( 'NONE', #1659, 5.000000000000004441 ) ;
#12228 = VERTEX_POINT ( 'NONE', #5666 ) ;
#12229 = CIRCLE ( 'NONE', #10240, 0.2500000000000002220 ) ;
#12230 = DIRECTION ( 'NONE',  ( 0.000000000000000000, 0.5000000000000008882, -0.8660254037844381525 ) ) ;
#12231 = ORIENTED_EDGE ( 'NONE', *, *, #7727, .T. ) ;
#12232 = APPLICATION_CONTEXT ( 'automotive_design' ) ;
#12233 = LINE ( 'NONE', #11356, #9309 ) ;
#12234 = VERTEX_POINT ( 'NONE', #11333 ) ;
#12235 = CARTESIAN_POINT ( 'NONE',  ( -36.00000000000000711, 0.000000000000000000, 0.000000000000000000 ) ) ;
#12236 = EDGE_CURVE ( 'NONE', #11797, #3600, #6417, .T. ) ;
#12237 = CARTESIAN_POINT ( 'NONE',  ( -1.250000000000000000, -6.429618962271402616, -1.000000000000000000 ) ) ;
#12238 = LINE ( 'NONE', #8567, #8762 ) ;
#12239 = CARTESIAN_POINT ( 'NONE',  ( 37.00000000000000711, -3.606021680338235225, -38.83193945118931367 ) ) ;
#12240 = EDGE_LOOP ( 'NONE', ( #3258, #11687, #10790, #2391 ) ) ;
#12241 = VERTEX_POINT ( 'NONE', #11282 ) ;
#12242 = CARTESIAN_POINT ( 'NONE',  ( 4.999999999999999112, 14.40062958310465469, -1.672489362011036595 ) ) ;
#12243 = VECTOR ( 'NONE', #2917, 1000.000000000000000 ) ;
#12244 =( NAMED_UNIT ( * ) SI_UNIT ( $, .STERADIAN. ) SOLID_ANGLE_UNIT ( ) );
#12245 = FACE_OUTER_BOUND ( 'NONE', #10500, .T. ) ;
#12246 = DIRECTION ( 'NONE',  ( 0.000000000000000000, 0.000000000000000000, -1.000000000000000000 ) ) ;
#12247 = ADVANCED_FACE ( 'NONE', ( #8485 ), #2851, .F. ) ;
#12248 = ORIENTED_EDGE ( 'NONE', *, *, #7478, .F. ) ;
#12249 = DIRECTION ( 'NONE',  ( 1.000000000000000000, 0.000000000000000000, 0.000000000000000000 ) ) ;
#12250 = EDGE_CURVE ( 'NONE', #6545, #6154, #10473, .T. ) ;
#12251 = VECTOR ( 'NONE', #6527, 1000.000000000000000 ) ;
#12252 = DIRECTION ( 'NONE',  ( 0.000000000000000000, 0.000000000000000000, 1.000000000000000000 ) ) ;
#12253 = FACE_OUTER_BOUND ( 'NONE', #11280, .T. ) ;
#12254 = VERTEX_POINT ( 'NONE', #12087 ) ;
#12255 = CARTESIAN_POINT ( 'NONE',  ( 0.000000000000000000, -1.561154383803364798, 20.18872947935930640 ) ) ;
#12256 = CARTESIAN_POINT ( 'NONE',  ( 4.999999999999999112, -21.74405275335762155, 15.58472803277448726 ) ) ;
#12257 = ORIENTED_EDGE ( 'NONE', *, *, #749, .T. ) ;
#12258 = CYLINDRICAL_SURFACE ( 'NONE', #10170, 9.600000000009600853 ) ;
#12259 = CARTESIAN_POINT ( 'NONE',  ( 51.00000000000000000, 0.000000000000000000, 0.000000000000000000 ) ) ;
#12260 = VERTEX_POINT ( 'NONE', #5418 ) ;
#12261 = DIRECTION ( 'NONE',  ( 1.000000000000000000, 0.000000000000000000, 0.000000000000000000 ) ) ;
#12262 = UNCERTAINTY_MEASURE_WITH_UNIT (LENGTH_MEASURE( 1.000000000000000082E-05 ), #7917, 'distance_accuracy_value', 'NONE');
#12263 = AXIS2_PLACEMENT_3D ( 'NONE', #7072, #9887, #252 ) ;
#12264 = ORIENTED_EDGE ( 'NONE', *, *, #9853, .F. ) ;
#12265 = EDGE_CURVE ( 'NONE', #11945, #7392, #10226, .T. ) ;
#12266 = EDGE_CURVE ( 'NONE', #9710, #908, #1255, .T. ) ;
#12267 = EDGE_CURVE ( 'NONE', #2661, #7918, #2450, .T. ) ;
#12268 = CARTESIAN_POINT ( 'NONE',  ( 4.999999999999999112, 0.000000000000000000, 0.000000000000000000 ) ) ;
#12269 = CARTESIAN_POINT ( 'NONE',  ( 51.00000000000000000, -3.499999999999998668, -38.49999999999998579 ) ) ;
#12270 = DIRECTION ( 'NONE',  ( 0.000000000000000000, 0.000000000000000000, 1.000000000000000000 ) ) ;
#12271 = CIRCLE ( 'NONE', #1502, 20.24900000002024569 ) ;
#12272 = DIRECTION ( 'NONE',  ( -1.000000000000000000, 0.000000000000000000, 0.000000000000000000 ) ) ;
#12273 = DIRECTION ( 'NONE',  ( -1.000000000000000000, -0.000000000000000000, -0.000000000000000000 ) ) ;
#12274 = ORIENTED_EDGE ( 'NONE', *, *, #10447, .T. ) ;
#12275 = ORIENTED_EDGE ( 'NONE', *, *, #9926, .T. ) ;
#12276 = DIRECTION ( 'NONE',  ( 0.000000000000000000, -0.4526840589413320126, 0.8916709834801178625 ) ) ;
#12277 = EDGE_LOOP ( 'NONE', ( #6510, #10281, #6910, #10900 ) ) ;
#12278 = CARTESIAN_POINT ( 'NONE',  ( 0.000000000000000000, 14.40062958310465469, -8.872489362018239234 ) ) ;
#12279 = DIRECTION ( 'NONE',  ( -1.000000000000000000, 0.000000000000000000, 0.000000000000000000 ) ) ;
#12280 = EDGE_CURVE ( 'NONE', #7137, #710, #11631, .T. ) ;
#12281 = ORIENTED_EDGE ( 'NONE', *, *, #10127, .F. ) ;
#12282 = DIRECTION ( 'NONE',  ( -1.000000000000000000, -0.000000000000000000, -0.000000000000000000 ) ) ;
#12283 = DIRECTION ( 'NONE',  ( 0.000000000000000000, 0.000000000000000000, 1.000000000000000000 ) ) ;
#12284 = ORIENTED_EDGE ( 'NONE', *, *, #3476, .F. ) ;
#12285 = ORIENTED_EDGE ( 'NONE', *, *, #8931, .T. ) ;
#12286 = CARTESIAN_POINT ( 'NONE',  ( 16.55500000000001393, 0.000000000000000000, 2.500000000000000444 ) ) ;
#12287 = CARTESIAN_POINT ( 'NONE',  ( 0.000000000000000000, -4.576198416197435392, 26.60936692326689013 ) ) ;
#12288 = LINE ( 'NONE', #3373, #9804 ) ;
#12289 = VERTEX_POINT ( 'NONE', #3601 ) ;
#12290 = CARTESIAN_POINT ( 'NONE',  ( 0.000000000000000000, 18.05452603534165945, 9.168210874537644273 ) ) ;
#12291 = ORIENTED_EDGE ( 'NONE', *, *, #7325, .F. ) ;
#12292 = FILL_AREA_STYLE ('',( #864 ) ) ;
#12293 = EDGE_CURVE ( 'NONE', #7624, #6970, #9447, .T. ) ;
#12294 = CARTESIAN_POINT ( 'NONE',  ( -26.00000000000000355, 30.00000000000000711, -19.99999999999998934 ) ) ;
#12295 = ORIENTED_EDGE ( 'NONE', *, *, #2819, .T. ) ;
#12296 = DIRECTION ( 'NONE',  ( 0.000000000000000000, 1.000000000000000000, 0.000000000000000000 ) ) ;
#12297 = CARTESIAN_POINT ( 'NONE',  ( 0.000000000000000000, 1.676853263448085052, -14.14998813191267857 ) ) ;
#12298 = FACE_OUTER_BOUND ( 'NONE', #8243, .T. ) ;
#12299 = CARTESIAN_POINT ( 'NONE',  ( 4.999999999999999112, -2.791921004064401579, 22.37914155802284100 ) ) ;
#12300 = ORIENTED_EDGE ( 'NONE', *, *, #1716, .T. ) ;
#12301 = EDGE_LOOP ( 'NONE', ( #12188, #1691, #8424, #10578 ) ) ;
#12302 = CARTESIAN_POINT ( 'NONE',  ( 0.000000000000000000, 0.5192545390863916310, 0.000000000000000000 ) ) ;
#12303 = CARTESIAN_POINT ( 'NONE',  ( 0.000000000000000000, 18.05452603534179090, -9.168210874537381372 ) ) ;
#12304 = CARTESIAN_POINT ( 'NONE',  ( 4.999999999999999112, 0.000000000000000000, 0.000000000000000000 ) ) ;
#12305 = ORIENTED_EDGE ( 'NONE', *, *, #2405, .F. ) ;
#12306 = CARTESIAN_POINT ( 'NONE',  ( 2.500000000000000000, 2.357898499370433054, -1.951563910473907981E-15 ) ) ;
#12307 = CARTESIAN_POINT ( 'NONE',  ( 4.999999999999999112, 22.37914155802285876, 6.808078995945277434 ) ) ;
#12308 = CARTESIAN_POINT ( 'NONE',  ( -36.00000000000000000, 7.347880794884118750E-16, 5.999999999999999112 ) ) ;
#12309 = EDGE_CURVE ( 'NONE', #10868, #3985, #12023, .T. ) ;
#12310 = DIRECTION ( 'NONE',  ( 0.000000000000000000, 0.000000000000000000, 1.000000000000000000 ) ) ;
#12311 = DIRECTION ( 'NONE',  ( 0.000000000000000000, 0.000000000000000000, -1.000000000000000000 ) ) ;
#12312 = ORIENTED_EDGE ( 'NONE', *, *, #10658, .T. ) ;
#12313 = EDGE_CURVE ( 'NONE', #10885, #11016, #7421, .T. ) ;
#12314 = CARTESIAN_POINT ( 'NONE',  ( 45.00000000000000000, 0.000000000000000000, 0.000000000000000000 ) ) ;
#12315 = DIRECTION ( 'NONE',  ( 0.000000000000000000, 0.000000000000000000, 1.000000000000000000 ) ) ;
#12316 = ORIENTED_EDGE ( 'NONE', *, *, #9838, .F. ) ;
#12317 = CARTESIAN_POINT ( 'NONE',  ( 0.5590169943749477843, 0.000000000000000000, 0.000000000000000000 ) ) ;
#12318 = ORIENTED_EDGE ( 'NONE', *, *, #3518, .F. ) ;
#12319 = DIRECTION ( 'NONE',  ( 0.000000000000000000, 0.000000000000000000, 1.000000000000000000 ) ) ;
#12320 = CARTESIAN_POINT ( 'NONE',  ( 50.00005079999999680, 0.000000000000000000, 0.000000000000000000 ) ) ;
#12321 = CARTESIAN_POINT ( 'NONE',  ( 36.00000000000000000, 30.00000000000000711, 20.00000000000001066 ) ) ;
#12322 = ADVANCED_FACE ( 'NONE', ( #2965 ), #29, .F. ) ;
#12323 = CARTESIAN_POINT ( 'NONE',  ( 70.79898987322334847, -3.499999999999998668, -45.49999999999998579 ) ) ;
#12324 = CARTESIAN_POINT ( 'NONE',  ( 0.000000000000000000, 8.035066368449411911, -14.88411597386720508 ) ) ;
#12325 = ORIENTED_EDGE ( 'NONE', *, *, #7477, .F. ) ;
#12327 = ADVANCED_FACE ( 'NONE', ( #10718 ), #3966, .T. ) ;
#12326 = EDGE_LOOP ( 'NONE', ( #6741, #561, #10641, #3016 ) ) ;
#12328 = EDGE_CURVE ( 'NONE', #1101, #6684, #2915, .T. ) ;
#12329 = LINE ( 'NONE', #10285, #4452 ) ;
#12330 = AXIS2_PLACEMENT_3D ( 'NONE', #2638, #12121, #5278 ) ;
#12331 = ADVANCED_FACE ( 'NONE', ( #5969 ), #7789, .T. ) ;
#12332 = ORIENTED_EDGE ( 'NONE', *, *, #2651, .T. ) ;
#12333 = CARTESIAN_POINT ( 'NONE',  ( 37.00000000000000711, 4.769696007084728073, -1.500000000000000444 ) ) ;
#12334 = APPLICATION_PROTOCOL_DEFINITION ( 'draft international standard', 'automotive_design', 1998, #11588 ) ;
#12335 = ORIENTED_EDGE ( 'NONE', *, *, #4712, .F. ) ;
#12336 = CARTESIAN_POINT ( 'NONE',  ( -1.399999999999999689, 0.000000000000000000, 0.000000000000000000 ) ) ;
#12337 = CARTESIAN_POINT ( 'NONE',  ( 0.000000000000000000, -8.527191590520994069, -11.41582255376081889 ) ) ;
#12338 = AXIS2_PLACEMENT_3D ( 'NONE', #6990, #6061, #9810 ) ;
#12339 = CIRCLE ( 'NONE', #11739, 4.799999999999999822 ) ;
#12340 = ORIENTED_EDGE ( 'NONE', *, *, #10594, .T. ) ;
#12341 = ORIENTED_EDGE ( 'NONE', *, *, #6845, .F. ) ;
#12342 = DIRECTION ( 'NONE',  ( 0.000000000000000000, 0.000000000000000000, -1.000000000000000000 ) ) ;
#12343 = LINE ( 'NONE', #5925, #7015 ) ;
#12344 = PLANE ( 'NONE',  #1621 ) ;
#12345 = CARTESIAN_POINT ( 'NONE',  ( 36.00000000000000711, 12.50000000000000000, -41.99999999999999289 ) ) ;
#12346 = ORIENTED_EDGE ( 'NONE', *, *, #3413, .T. ) ;
#12347 = CARTESIAN_POINT ( 'NONE',  ( 4.999999999999999112, 0.000000000000000000, 0.000000000000000000 ) ) ;
#12348 = CIRCLE ( 'NONE', #7376, 21.00000000002100009 ) ;
#12349 = ORIENTED_EDGE ( 'NONE', *, *, #5258, .T. ) ;
#12350 = CIRCLE ( 'NONE', #9179, 5.000000000000000000 ) ;
#12351 = SURFACE_STYLE_FILL_AREA ( #10299 ) ;
#12352 = DIRECTION ( 'NONE',  ( -1.000000000000000000, 0.000000000000000000, -0.000000000000000000 ) ) ;
#12353 = NEXT_ASSEMBLY_USAGE_OCCURRENCE ( 'NAUO1', ' ', ' ', #11287, #8872, $ ) ;
#12354 = NEXT_ASSEMBLY_USAGE_OCCURRENCE ( 'NAUO2', ' ', ' ', #11287, #3130, $ ) ;
#12355 = NEXT_ASSEMBLY_USAGE_OCCURRENCE ( 'NAUO3', ' ', ' ', #11287, #7937, $ ) ;
#12356 = NEXT_ASSEMBLY_USAGE_OCCURRENCE ( 'NAUO4', ' ', ' ', #11287, #8707, $ ) ;
#12357 = NEXT_ASSEMBLY_USAGE_OCCURRENCE ( 'NAUO5', ' ', ' ', #11287, #7554, $ ) ;
#12358 = NEXT_ASSEMBLY_USAGE_OCCURRENCE ( 'NAUO6', ' ', ' ', #11287, #5170, $ ) ;
#12359 = NEXT_ASSEMBLY_USAGE_OCCURRENCE ( 'NAUO7', ' ', ' ', #11287, #9994, $ ) ;
#12360 = NEXT_ASSEMBLY_USAGE_OCCURRENCE ( 'NAUO8', ' ', ' ', #11287, #7402, $ ) ;
#12361 = NEXT_ASSEMBLY_USAGE_OCCURRENCE ( 'NAUO9', ' ', ' ', #11287, #11668, $ ) ;
#12362 = NEXT_ASSEMBLY_USAGE_OCCURRENCE ( 'NAUO10', ' ', ' ', #11287, #11668, $ ) ;
#12363 = NEXT_ASSEMBLY_USAGE_OCCURRENCE ( 'NAUO11', ' ', ' ', #11287, #9994, $ ) ;
#12364 = NEXT_ASSEMBLY_USAGE_OCCURRENCE ( 'NAUO12', ' ', ' ', #11287, #9994, $ ) ;
#12365 = NEXT_ASSEMBLY_USAGE_OCCURRENCE ( 'NAUO13', ' ', ' ', #11287, #11668, $ ) ;
#12366 = NEXT_ASSEMBLY_USAGE_OCCURRENCE ( 'NAUO14', ' ', ' ', #11287, #9774, $ ) ;
#12367 = NEXT_ASSEMBLY_USAGE_OCCURRENCE ( 'NAUO15', ' ', ' ', #11287, #7780, $ ) ;
#12368 = NEXT_ASSEMBLY_USAGE_OCCURRENCE ( 'NAUO16', ' ', ' ', #11287, #7780, $ ) ;
#12369 = NEXT_ASSEMBLY_USAGE_OCCURRENCE ( 'NAUO17', ' ', ' ', #11287, #2198, $ ) ;
#12370 = NEXT_ASSEMBLY_USAGE_OCCURRENCE ( 'NAUO18', ' ', ' ', #11287, #6878, $ ) ;
#12371=COLOUR_RGB('Dark Blue',0.08,0.2,0.34);
#12372=FILL_AREA_STYLE_COLOUR('',#12371);
#12373=FILL_AREA_STYLE('',(#12372));
#12374=SURFACE_STYLE_FILL_AREA(#12373);
#12375=SURFACE_SIDE_STYLE('',(#12374));
#12376=SURFACE_STYLE_USAGE(.BOTH.,#12375);
#12377=PRESENTATION_STYLE_ASSIGNMENT((#12376));
#12378=COLOUR_RGB('Light Blue',0.38,0.62,0.78);
#12379=FILL_AREA_STYLE_COLOUR('',#12378);
#12380=FILL_AREA_STYLE('',(#12379));
#12381=SURFACE_STYLE_FILL_AREA(#12380);
#12382=SURFACE_SIDE_STYLE('',(#12381));
#12383=SURFACE_STYLE_USAGE(.BOTH.,#12382);
#12384=PRESENTATION_STYLE_ASSIGNMENT((#12383));
#12385=COLOUR_RGB('Sky Blue',0.24,0.69,0.87);
#12386=FILL_AREA_STYLE_COLOUR('',#12385);
#12387=FILL_AREA_STYLE('',(#12386));
#12388=SURFACE_STYLE_FILL_AREA(#12387);
#12389=SURFACE_SIDE_STYLE('',(#12388));
#12390=SURFACE_STYLE_USAGE(.BOTH.,#12389);
#12391=PRESENTATION_STYLE_ASSIGNMENT((#12390));
#12392=COLOUR_RGB('Grey',0.48,0.52,0.57);
#12393=FILL_AREA_STYLE_COLOUR('',#12392);
#12394=FILL_AREA_STYLE('',(#12393));
#12395=SURFACE_STYLE_FILL_AREA(#12394);
#12396=SURFACE_SIDE_STYLE('',(#12395));
#12397=SURFACE_STYLE_USAGE(.BOTH.,#12396);
#12398=PRESENTATION_STYLE_ASSIGNMENT((#12397));
#12399=COLOUR_RGB('Black',0.12,0.14,0.17);
#12400=FILL_AREA_STYLE_COLOUR('',#12399);
#12401=FILL_AREA_STYLE('',(#12400));
#12402=SURFACE_STYLE_FILL_AREA(#12401);
#12403=SURFACE_SIDE_STYLE('',(#12402));
#12404=SURFACE_STYLE_USAGE(.BOTH.,#12403);
#12405=PRESENTATION_STYLE_ASSIGNMENT((#12404));
#12406=COLOUR_RGB('Off White',0.89,0.88,0.83);
#12407=FILL_AREA_STYLE_COLOUR('',#12406);
#12408=FILL_AREA_STYLE('',(#12407));
#12409=SURFACE_STYLE_FILL_AREA(#12408);
#12410=SURFACE_SIDE_STYLE('',(#12409));
#12411=SURFACE_STYLE_USAGE(.BOTH.,#12410);
#12412=PRESENTATION_STYLE_ASSIGNMENT((#12411));
ENDSEC;
END-ISO-10303-21;
